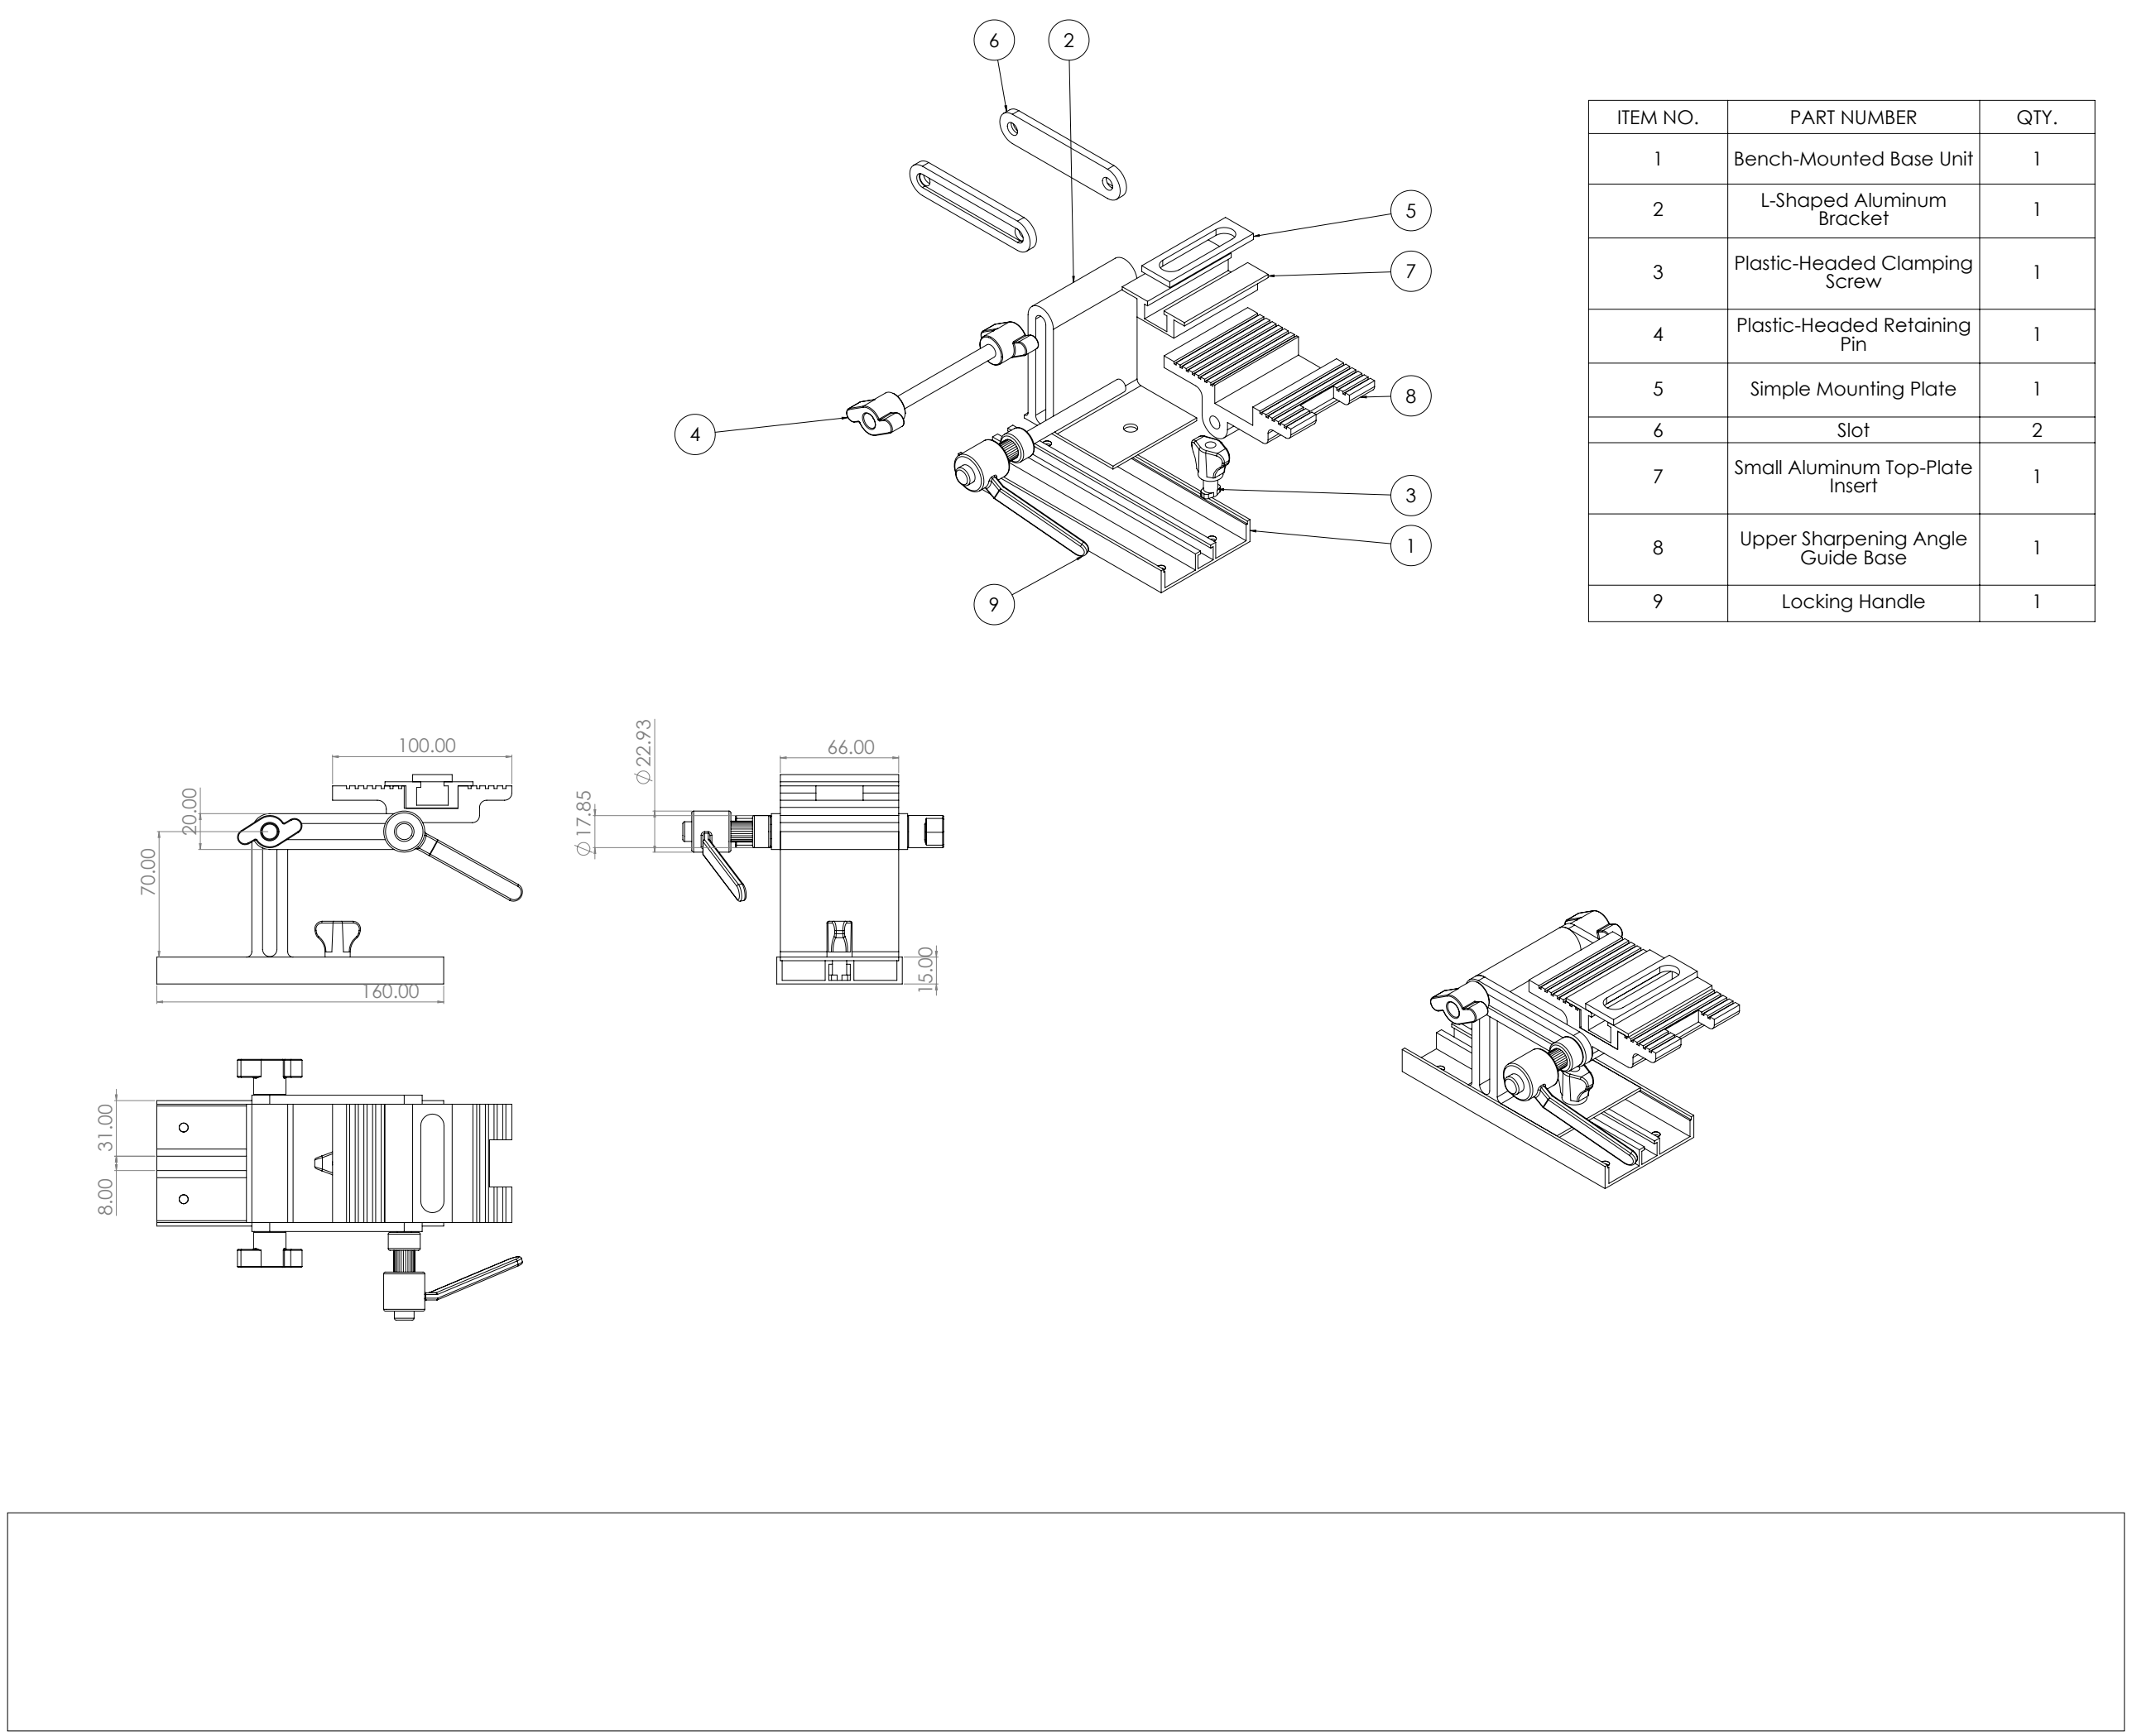
ISO-10303-21;
HEADER;
FILE_DESCRIPTION (('STEP AP214'),
    '1' );
FILE_NAME ('MAS-317',
    '2026-10-24T21:31:31',
    ( '' ),
    ( '' ),
    'SwSTEP 2.0',
    'SolidWorks 2025',
    '' );
FILE_SCHEMA (( 'AUTOMOTIVE_DESIGN' ));
ENDSEC;

DATA;
#1 = AXIS2_PLACEMENT_3D ( 'NONE', #1022, #12813, #2258 ) ;
#2 = CARTESIAN_POINT ( 'NONE',  ( 58.00000000000000711, -2.249290599286309256, 86.40005259842790508 ) ) ;
#3 = CARTESIAN_POINT ( 'NONE',  ( 58.00000000000000711, -2.249290599286309256, 86.40005259842790508 ) ) ;
#4 = EDGE_CURVE ( 'NONE', #12159, #10942, #11483, .T. ) ;
#5 = EDGE_LOOP ( 'NONE', ( #6099, #8745, #4266, #9000 ) ) ;
#6 = LINE ( 'NONE', #11694, #4610 ) ;
#7 = CARTESIAN_POINT ( 'NONE',  ( 64.16497654487091040, -11.91588057969686965, 72.65167857827074727 ) ) ;
#8 = EDGE_CURVE ( 'NONE', #12161, #11292, #4111, .T. ) ;
#9 = CARTESIAN_POINT ( 'NONE',  ( 27.62489819272141389, -52.24929059928630437, 4.899481419381555014 ) ) ;
#10 = CARTESIAN_POINT ( 'NONE',  ( 23.72005712271873890, -60.79495753911086098, 6.390225278796987318 ) ) ;
#11 = EDGE_LOOP ( 'NONE', ( #10298, #886, #9841, #4831, #11174, #11784, #1803, #163, #11627, #11601, #5374, #7472, #708, #12281, #12120, #14505 ) ) ;
#12 = EDGE_CURVE ( 'NONE', #11983, #7767, #13962, .T. ) ;
#13 = LINE ( 'NONE', #7011, #3647 ) ;
#14 = VECTOR ( 'NONE', #2004, 1000.000000000000000 ) ;
#15 = ORIENTED_EDGE ( 'NONE', *, *, #6036, .T. ) ;
#16 = CARTESIAN_POINT ( 'NONE',  ( 58.00000000000000711, -2.249290599286311032, 36.00000000000012079 ) ) ;
#17 = DIRECTION ( 'NONE',  ( -1.000000000000000000, 0.000000000000000000, 0.000000000000000000 ) ) ;
#18 = ADVANCED_FACE ( 'NONE', ( #1362 ), #5786, .T. ) ;
#19 = ADVANCED_FACE ( 'NONE', ( #7663 ), #4110, .F. ) ;
#20 = VERTEX_POINT ( 'NONE', #5429 ) ;
#21 =( NAMED_UNIT ( * ) PLANE_ANGLE_UNIT ( ) SI_UNIT ( $, .RADIAN. ) );
#22 = DIRECTION ( 'NONE',  ( 0.000000000000000000, 0.000000000000000000, -1.000000000000000000 ) ) ;
#23 = FACE_OUTER_BOUND ( 'NONE', #14250, .T. ) ;
#24 = ORIENTED_EDGE ( 'NONE', *, *, #9295, .T. ) ;
#25 = LINE ( 'NONE', #2406, #7510 ) ;
#26 = DIRECTION ( 'NONE',  ( -0.8746197071345572782, 0.4848096202550659650, 1.387778780781444256E-14 ) ) ;
#27 = ADVANCED_FACE ( 'NONE', ( #435 ), #1875, .T. ) ;
#28 = FACE_OUTER_BOUND ( 'NONE', #3772, .T. ) ;
#29 = DIRECTION ( 'NONE',  ( 1.000000000000000000, 0.000000000000000000, 0.000000000000000000 ) ) ;
#30 = EDGE_CURVE ( 'NONE', #1762, #13149, #4870, .T. ) ;
#31 = CARTESIAN_POINT ( 'NONE',  ( -24.73111225919155132, -6.857688092579577344, -47.70917337021941762 ) ) ;
#32 = FACE_OUTER_BOUND ( 'NONE', #11110, .T. ) ;
#33 = ADVANCED_FACE ( 'NONE', ( #12199 ), #9834, .F. ) ;
#34 = ORIENTED_EDGE ( 'NONE', *, *, #2571, .T. ) ;
#35 = CIRCLE ( 'NONE', #11822, 8.924024642120691908 ) ;
#36 = DIRECTION ( 'NONE',  ( 0.000000000000000000, 0.000000000000000000, 1.000000000000000000 ) ) ;
#37 = ORIENTED_EDGE ( 'NONE', *, *, #2232, .F. ) ;
#38 = FACE_OUTER_BOUND ( 'NONE', #6545, .T. ) ;
#39 = DIRECTION ( 'NONE',  ( -0.3020115420618247892, 0.1674077314120183957, -0.9384901064608620613 ) ) ;
#40 = CARTESIAN_POINT ( 'NONE',  ( 62.00000000000001421, -2.249290599286311032, -49.31370849898490150 ) ) ;
#41 = LINE ( 'NONE', #2497, #6085 ) ;
#42 = AXIS2_PLACEMENT_3D ( 'NONE', #10885, #14351, #11948 ) ;
#43 = CARTESIAN_POINT ( 'NONE',  ( 116.3214526938479025, -39.15081599364015119, 53.46824312087640863 ) ) ;
#44 = AXIS2_PLACEMENT_3D ( 'NONE', #5649, #10264, #10339 ) ;
#45 = CIRCLE ( 'NONE', #9384, 9.000000000000001776 ) ;
#46 = PLANE ( 'NONE',  #3626 ) ;
#47 = CARTESIAN_POINT ( 'NONE',  ( 46.91810375148135392, 21.75070940071322667, 139.1143251403882459 ) ) ;
#48 = CARTESIAN_POINT ( 'NONE',  ( -24.79038709231510040, -6.757381419356298657, 47.62582736825572738 ) ) ;
#49 = CARTESIAN_POINT ( 'NONE',  ( -2.016677571526633510E-15, 23.25070940071368497, -33.00000000000012790 ) ) ;
#50 = LINE ( 'NONE', #1350, #13702 ) ;
#51 = ORIENTED_EDGE ( 'NONE', *, *, #11161, .F. ) ;
#52 = CARTESIAN_POINT ( 'NONE',  ( 8.091875466796944139, -56.52532528994245808, 1.842181053809107238 ) ) ;
#53 = VECTOR ( 'NONE', #9034, 1000.000000000000000 ) ;
#54 = VECTOR ( 'NONE', #13573, 1000.000000000000000 ) ;
#55 = EDGE_CURVE ( 'NONE', #10251, #7651, #14932, .T. ) ;
#56 = VERTEX_POINT ( 'NONE', #6360 ) ;
#57 = LINE ( 'NONE', #11745, #6919 ) ;
#58 = VECTOR ( 'NONE', #2580, 1000.000000000000000 ) ;
#59 = VERTEX_POINT ( 'NONE', #10047 ) ;
#60 = VERTEX_POINT ( 'NONE', #14733 ) ;
#61 = CARTESIAN_POINT ( 'NONE',  ( 65.61438479068812057, -11.78561916032472823, 75.96106737140233633 ) ) ;
#62 = CARTESIAN_POINT ( 'NONE',  ( 114.6731053250840233, 21.75070940071369918, 139.1143251403882459 ) ) ;
#63 = DIRECTION ( 'NONE',  ( 0.000000000000000000, 1.734723475976817547E-15, -1.000000000000000000 ) ) ;
#64 = MECHANICAL_DESIGN_GEOMETRIC_PRESENTATION_REPRESENTATION (  '', ( #7176 ), #14543 ) ;
#65 = VERTEX_POINT ( 'NONE', #11047 ) ;
#66 = VECTOR ( 'NONE', #7622, 1000.000000000000000 ) ;
#67 = CARTESIAN_POINT ( 'NONE',  ( 8.466388902489018875, -58.63671300496866223, -1.826958383930360919 ) ) ;
#68 = PLANE ( 'NONE',  #7695 ) ;
#69 = LINE ( 'NONE', #10606, #11985 ) ;
#70 = CIRCLE ( 'NONE', #4772, 3.000000000000000888 ) ;
#71 = ORIENTED_EDGE ( 'NONE', *, *, #11240, .T. ) ;
#72 = VERTEX_POINT ( 'NONE', #721 ) ;
#73 = EDGE_CURVE ( 'NONE', #927, #9462, #501, .T. ) ;
#74 = EDGE_CURVE ( 'NONE', #5063, #10163, #11263, .T. ) ;
#75 = PLANE ( 'NONE',  #1648 ) ;
#76 = ORIENTED_EDGE ( 'NONE', *, *, #9899, .T. ) ;
#77 = VERTEX_POINT ( 'NONE', #4338 ) ;
#78 = CARTESIAN_POINT ( 'NONE',  ( 10.10272221478045296, -60.61171897230391892, -3.004288329735573804 ) ) ;
#79 = ORIENTED_EDGE ( 'NONE', *, *, #10646, .T. ) ;
#80 = CIRCLE ( 'NONE', #11854, 0.5000000000000000000 ) ;
#81 = VERTEX_POINT ( 'NONE', #9278 ) ;
#82 = B_SPLINE_CURVE_WITH_KNOTS ( 'NONE', 3,
 ( #2803, #3028, #1934, #12180, #8712, #1641, #3094, #13404, #11248, #10961, #410, #7643, #1857, #1791, #7796, #12259, #700, #6406 ),
 .UNSPECIFIED., .F., .F.,
 ( 4, 2, 2, 2, 2, 2, 2, 2, 4 ),
 ( 0.000000000000000000, 0.0007600084067931386217, 0.001520016813586277243, 0.002280025220379415865, 0.003040033627172554487, 0.003800042033965693108, 0.004560050440758831730, 0.005320058847551970352, 0.006080067254345108974 ),
 .UNSPECIFIED. ) ;
#83 = CARTESIAN_POINT ( 'NONE',  ( -24.54250511040913096, 2.674312581063694516, -47.50000000000008527 ) ) ;
#84 = DIRECTION ( 'NONE',  ( -0.000000000000000000, 0.000000000000000000, -1.000000000000000000 ) ) ;
#85 = ORIENTED_EDGE ( 'NONE', *, *, #4287, .T. ) ;
#86 = VECTOR ( 'NONE', #1332, 1000.000000000000000 ) ;
#87 = LINE ( 'NONE', #2465, #13317 ) ;
#88 = FACE_OUTER_BOUND ( 'NONE', #4233, .T. ) ;
#89 = ORIENTED_EDGE ( 'NONE', *, *, #5308, .T. ) ;
#90 = DIRECTION ( 'NONE',  ( 0.000000000000000000, 0.000000000000000000, -1.000000000000000000 ) ) ;
#91 = CARTESIAN_POINT ( 'NONE',  ( 32.77533487224304309, -57.91121052158847249, 2.751677492798574320 ) ) ;
#92 = APPLICATION_CONTEXT ( 'automotive_design' ) ;
#93 = CARTESIAN_POINT ( 'NONE',  ( -30.80945343098651890, -5.389243620311580329, -57.50000000000012079 ) ) ;
#94 = ORIENTED_EDGE ( 'NONE', *, *, #8937, .F. ) ;
#95 = VECTOR ( 'NONE', #9996, 1000.000000000000000 ) ;
#96 = DIRECTION ( 'NONE',  ( 0.9421718071228325497, 6.170304995646513309E-16, -0.3351302520855077849 ) ) ;
#97 = AXIS2_PLACEMENT_3D ( 'NONE', #6521, #12302, #1688 ) ;
#98 = ORIENTED_EDGE ( 'NONE', *, *, #8570, .T. ) ;
#99 = CARTESIAN_POINT ( 'NONE',  ( 40.00000000000001421, -72.24929059928631148, -32.99999999999982947 ) ) ;
#100 = DIRECTION ( 'NONE',  ( -0.8746197071345569451, 0.4848096202550666312, 0.000000000000000000 ) ) ;
#101 = ORIENTED_EDGE ( 'NONE', *, *, #8706, .F. ) ;
#102 = ORIENTED_EDGE ( 'NONE', *, *, #10358, .T. ) ;
#103 =( NAMED_UNIT ( * ) PLANE_ANGLE_UNIT ( ) SI_UNIT ( $, .RADIAN. ) );
#104 = CARTESIAN_POINT ( 'NONE',  ( 9.074528850127588697, -58.48798588983633095, 2.754379989674547780 ) ) ;
#105 = LINE ( 'NONE', #10640, #5976 ) ;
#106 = ORIENTED_EDGE ( 'NONE', *, *, #4616, .T. ) ;
#107 = CARTESIAN_POINT ( 'NONE',  ( -9.038486528834313916, 1.949452350488303454, -47.50000000626571506 ) ) ;
#108 = DIRECTION ( 'NONE',  ( 0.000000000000000000, 0.000000000000000000, 1.000000000000000000 ) ) ;
#109 = DIRECTION ( 'NONE',  ( 0.000000000000000000, 1.000000000000000000, 0.000000000000000000 ) ) ;
#110 = LINE ( 'NONE', #11941, #4147 ) ;
#111 = FACE_OUTER_BOUND ( 'NONE', #10692, .T. ) ;
#112 = EDGE_CURVE ( 'NONE', #12771, #10151, #4658, .T. ) ;
#113 = CARTESIAN_POINT ( 'NONE',  ( 33.37135420079148673, -55.04126158147273884, -2.748788379873860599 ) ) ;
#114 = ORIENTED_EDGE ( 'NONE', *, *, #14825, .F. ) ;
#115 = EDGE_LOOP ( 'NONE', ( #13949, #4522, #9265, #7527 ) ) ;
#116 = CARTESIAN_POINT ( 'NONE',  ( 0.000000000000000000, 21.75070940071363168, 33.00000000000012790 ) ) ;
#117 = VERTEX_POINT ( 'NONE', #8210 ) ;
#118 = LINE ( 'NONE', #8565, #1013 ) ;
#119 = CARTESIAN_POINT ( 'NONE',  ( -3.190546569013415379, 0.8906624217387615339, -57.50000000000012079 ) ) ;
#120 = LINE ( 'NONE', #8431, #11123 ) ;
#121 = CARTESIAN_POINT ( 'NONE',  ( 54.21883389619742388, -5.612936290787406968, 62.84860122826521689 ) ) ;
#122 = EDGE_CURVE ( 'NONE', #12222, #13012, #6096, .T. ) ;
#123 = ADVANCED_FACE ( 'NONE', ( #3273 ), #5820, .F. ) ;
#124 = CARTESIAN_POINT ( 'NONE',  ( 69.30309607900824176, -4.171217477998490075, 76.23845400177138742 ) ) ;
#125 = CARTESIAN_POINT ( 'NONE',  ( 13.86797143582180780, -68.67521603617343828, 4.260811380360699729 ) ) ;
#126 = DIRECTION ( 'NONE',  ( 0.000000000000000000, 0.000000000000000000, 1.000000000000000000 ) ) ;
#127 = CARTESIAN_POINT ( 'NONE',  ( -25.21252699837112132, -6.998437922861948657, 48.50000000000011369 ) ) ;
#128 = FACE_BOUND ( 'NONE', #8065, .T. ) ;
#129 = CARTESIAN_POINT ( 'NONE',  ( 30.58625090343030806, -52.41844408481608752, 2.861639392408844351 ) ) ;
#130 = ORIENTED_EDGE ( 'NONE', *, *, #11606, .T. ) ;
#131 = CARTESIAN_POINT ( 'NONE',  ( 20.86173033120691045, -53.24929059928630437, 0.000000000000000000 ) ) ;
#132 = ORIENTED_EDGE ( 'NONE', *, *, #1705, .F. ) ;
#133 = DIRECTION ( 'NONE',  ( 1.000000000000000000, 0.000000000000000000, 0.000000000000000000 ) ) ;
#134 = ORIENTED_EDGE ( 'NONE', *, *, #9339, .T. ) ;
#135 = ORIENTED_EDGE ( 'NONE', *, *, #2741, .T. ) ;
#136 = CARTESIAN_POINT ( 'NONE',  ( 64.12616288941416087, -11.93994285747185913, 75.47114622899779590 ) ) ;
#137 = CARTESIAN_POINT ( 'NONE',  ( 65.80512781895316721, -6.575743597179694255, 39.50000000000012790 ) ) ;
#138 = CARTESIAN_POINT ( 'NONE',  ( 48.00000000000000000, -2.249290599286307479, 139.1143251403882459 ) ) ;
#139 = CARTESIAN_POINT ( 'NONE',  ( 9.123957934261133218, -53.72645478541605257, 3.103403305059656336 ) ) ;
#140 = ADVANCED_FACE ( 'NONE', ( #6968 ), #10511, .T. ) ;
#141 = CARTESIAN_POINT ( 'NONE',  ( 59.31076468612580754, 2.638779099491020297, 60.61639468829817190 ) ) ;
#142 = CARTESIAN_POINT ( 'NONE',  ( 67.15257324181105503, -7.322644791425994448, 61.61639468829817190 ) ) ;
#143 = VERTEX_POINT ( 'NONE', #9046 ) ;
#144 = CARTESIAN_POINT ( 'NONE',  ( 65.51787304867481510, -10.90583193546819274, 77.18393887567587797 ) ) ;
#145 = ORIENTED_EDGE ( 'NONE', *, *, #4688, .T. ) ;
#146 = DIRECTION ( 'NONE',  ( -0.9744556954135545901, 0.2245798247307304318, 0.000000000000000000 ) ) ;
#147 = ORIENTED_EDGE ( 'NONE', *, *, #2886, .F. ) ;
#148 = LINE ( 'NONE', #14233, #12794 ) ;
#149 = AXIS2_PLACEMENT_3D ( 'NONE', #12314, #13325, #4001 ) ;
#150 = ORIENTED_EDGE ( 'NONE', *, *, #12236, .T. ) ;
#151 = CARTESIAN_POINT ( 'NONE',  ( -22.13891797369473480, 5.141277655368648780, -48.38337049880507834 ) ) ;
#152 = CARTESIAN_POINT ( 'NONE',  ( 65.93900958890544928, -0.9331851346922672708, 76.19766410831374515 ) ) ;
#153 = VERTEX_POINT ( 'NONE', #5752 ) ;
#154 = DIRECTION ( 'NONE',  ( -0.000000000000000000, 1.000000000000000000, -0.000000000000000000 ) ) ;
#155 = LINE ( 'NONE', #2612, #2752 ) ;
#156 = EDGE_LOOP ( 'NONE', ( #7728, #5694, #9406, #597 ) ) ;
#157 = EDGE_CURVE ( 'NONE', #531, #1580, #7972, .T. ) ;
#158 = ADVANCED_FACE ( 'NONE', ( #10353 ), #436, .F. ) ;
#159 = TOROIDAL_SURFACE ( 'NONE', #9985, 10.46463184759104870, 1.000000000000000000 ) ;
#160 = DIRECTION ( 'NONE',  ( -0.000000000000000000, -0.000000000000000000, -1.000000000000000000 ) ) ;
#161 = CARTESIAN_POINT ( 'NONE',  ( 42.07846078193830408, 21.75070940071319114, 139.1143251403882459 ) ) ;
#162 = DIRECTION ( 'NONE',  ( 0.000000000000000000, 0.000000000000000000, 1.000000000000000000 ) ) ;
#163 = ORIENTED_EDGE ( 'NONE', *, *, #14073, .T. ) ;
#164 = CARTESIAN_POINT ( 'NONE',  ( -24.34296084301338681, 2.966536634491813818, 47.54128347412125066 ) ) ;
#165 = EDGE_CURVE ( 'NONE', #11054, #3062, #11494, .T. ) ;
#166 = VERTEX_POINT ( 'NONE', #3346 ) ;
#167 = DIRECTION ( 'NONE',  ( -1.000000000000000000, 0.000000000000000000, 0.000000000000000000 ) ) ;
#168 =( NAMED_UNIT ( * ) PLANE_ANGLE_UNIT ( ) SI_UNIT ( $, .RADIAN. ) );
#169 = AXIS2_PLACEMENT_3D ( 'NONE', #4841, #13010, #2308 ) ;
#170 = VERTEX_POINT ( 'NONE', #13972 ) ;
#171 = VECTOR ( 'NONE', #13826, 1000.000000000000000 ) ;
#172 = LINE ( 'NONE', #1320, #11742 ) ;
#173 = CARTESIAN_POINT ( 'NONE',  ( 29.24198010098110245, -64.22824823034754615, 3.135769320951033112 ) ) ;
#174 = EDGE_CURVE ( 'NONE', #2378, #7934, #12219, .T. ) ;
#175 = CARTESIAN_POINT ( 'NONE',  ( -9.097850607046364502, 2.059891325575069043, -47.52616914649232172 ) ) ;
#176 = CARTESIAN_POINT ( 'NONE',  ( 13.73779544508787431, -66.12426320349668174, 4.110478850042866839 ) ) ;
#177 = AXIS2_PLACEMENT_3D ( 'NONE', #1271, #10901, #2354 ) ;
#178 = LINE ( 'NONE', #7254, #6578 ) ;
#179 = FACE_OUTER_BOUND ( 'NONE', #4257, .T. ) ;
#180 = CARTESIAN_POINT ( 'NONE',  ( 33.55553634841081845, -55.70626543767114214, 1.910065177037574946 ) ) ;
#181 = CIRCLE ( 'NONE', #13427, 4.505436745857433145 ) ;
#182 = FACE_OUTER_BOUND ( 'NONE', #8671, .T. ) ;
#183 = CIRCLE ( 'NONE', #7797, 6.484807146443463566 ) ;
#184 = ORIENTED_EDGE ( 'NONE', *, *, #4181, .F. ) ;
#185 = CARTESIAN_POINT ( 'NONE',  ( 121.8459904851758893, -37.63970102501964021, 53.02550872668530246 ) ) ;
#186 = EDGE_LOOP ( 'NONE', ( #1865, #4805, #14383, #1234 ) ) ;
#187 = CARTESIAN_POINT ( 'NONE',  ( 67.21328690825531282, 25.52935533987996664, 84.20452624982236500 ) ) ;
#188 = CARTESIAN_POINT ( 'NONE',  ( 18.24487436548682240, -53.24929059928630437, 6.492462156583986399 ) ) ;
#189 = PRODUCT_DEFINITION_FORMATION_WITH_SPECIFIED_SOURCE ( 'ANY', '', #5935, .NOT_KNOWN. ) ;
#190 = DIRECTION ( 'NONE',  ( -1.000000000000000000, -0.000000000000000000, -0.000000000000000000 ) ) ;
#191 = DIRECTION ( 'NONE',  ( 0.000000000000000000, 0.000000000000000000, 1.000000000000000000 ) ) ;
#192 = CIRCLE ( 'NONE', #14918, 0.7892041907098250597 ) ;
#193 = TOROIDAL_SURFACE ( 'NONE', #8776, 5.165819364273509073, 0.5000000000000000000 ) ;
#194 = CARTESIAN_POINT ( 'NONE',  ( -16.99999999999998579, -2.249290599286303927, 33.00000000000012790 ) ) ;
#195 = CARTESIAN_POINT ( 'NONE',  ( 65.61529858912808777, -10.82031860958136704, 71.19766410831375936 ) ) ;
#196 = EDGE_CURVE ( 'NONE', #211, #4051, #4578, .T. ) ;
#197 = DIRECTION ( 'NONE',  ( 1.000000000000000000, 0.000000000000000000, 0.000000000000000000 ) ) ;
#198 = CARTESIAN_POINT ( 'NONE',  ( -25.01741698508091005, -6.338425579613558014, 48.00000000000010658 ) ) ;
#199 = AXIS2_PLACEMENT_3D ( 'NONE', #2893, #5282, #2974 ) ;
#200 = CLOSED_SHELL ( 'NONE', ( #3830, #2727, #245, #8105, #11848, #11362, #3505, #1082, #828, #2082, #3069, #6755, #8169, #6132, #6771, #8839, #9223 ) ) ;
#201 = CARTESIAN_POINT ( 'NONE',  ( 32.69801279946867112, -53.84541978742783641, 3.062363702218897643 ) ) ;
#202 = ADVANCED_FACE ( 'NONE', ( #3509 ), #12825, .F. ) ;
#203 = VECTOR ( 'NONE', #10665, 1000.000000000000000 ) ;
#204 = ORIENTED_EDGE ( 'NONE', *, *, #247, .F. ) ;
#205 = ADVANCED_FACE ( 'NONE', ( #8045 ), #8050, .F. ) ;
#206 = AXIS2_PLACEMENT_3D ( 'NONE', #6103, #12884, #8338 ) ;
#207 = EDGE_CURVE ( 'NONE', #5032, #7204, #4344, .T. ) ;
#208 = DIRECTION ( 'NONE',  ( -2.102695122396130409E-16, 0.000000000000000000, -1.000000000000000000 ) ) ;
#209 = ORIENTED_EDGE ( 'NONE', *, *, #14302, .F. ) ;
#210 = CARTESIAN_POINT ( 'NONE',  ( 1.004339113574583608, 0.8906624217387615339, -48.00000000000012079 ) ) ;
#211 = VERTEX_POINT ( 'NONE', #3190 ) ;
#212 = PLANE ( 'NONE',  #10140 ) ;
#213 = DIRECTION ( 'NONE',  ( 0.000000000000000000, 0.000000000000000000, -1.000000000000000000 ) ) ;
#214 = EDGE_CURVE ( 'NONE', #14442, #11277, #7315, .T. ) ;
#215 = CIRCLE ( 'NONE', #445, 0.5000000000000000000 ) ;
#216 = LINE ( 'NONE', #3742, #12117 ) ;
#217 = DIRECTION ( 'NONE',  ( -0.000000000000000000, 0.000000000000000000, 1.000000000000000000 ) ) ;
#218 = PLANE ( 'NONE',  #1793 ) ;
#219 = DIRECTION ( 'NONE',  ( 0.8420378618367728718, 0.5394184268574404584, -0.000000000000000000 ) ) ;
#220 = ORIENTED_EDGE ( 'NONE', *, *, #12965, .T. ) ;
#221 = EDGE_LOOP ( 'NONE', ( #14150, #12830, #6180, #1820 ) ) ;
#222 = EDGE_CURVE ( 'NONE', #13907, #15116, #14885, .T. ) ;
#223 = DIRECTION ( 'NONE',  ( 9.912705577010325549E-17, -1.734723475976817547E-15, 1.000000000000000000 ) ) ;
#224 = ORIENTED_EDGE ( 'NONE', *, *, #5040, .T. ) ;
#225 = ORIENTED_EDGE ( 'NONE', *, *, #12393, .F. ) ;
#226 = CYLINDRICAL_SURFACE ( 'NONE', #7156, 10.15857703477299978 ) ;
#227 = ORIENTED_EDGE ( 'NONE', *, *, #14224, .F. ) ;
#228 = CARTESIAN_POINT ( 'NONE',  ( 12.36791015745245836, -52.24929059928630437, 3.199931146564424012 ) ) ;
#229 = AXIS2_PLACEMENT_3D ( 'NONE', #14012, #3468, #10624 ) ;
#230 = EDGE_CURVE ( 'NONE', #13103, #13525, #1896, .T. ) ;
#231 = EDGE_LOOP ( 'NONE', ( #10918, #12061, #5408, #5048 ) ) ;
#232 = DIRECTION ( 'NONE',  ( 0.8746197071345569451, -0.4848096202550666312, 0.000000000000000000 ) ) ;
#233 = CARTESIAN_POINT ( 'NONE',  ( 63.00747169918385993, -1.516790343742004055, 62.84860122826521689 ) ) ;
#234 = ORIENTED_EDGE ( 'NONE', *, *, #174, .T. ) ;
#235 = LINE ( 'NONE', #14317, #9148 ) ;
#236 = CARTESIAN_POINT ( 'NONE',  ( 118.0000000000000568, 2.046973701652633381E-13, 13.14990448602693007 ) ) ;
#237 = ORIENTED_EDGE ( 'NONE', *, *, #6908, .T. ) ;
#238 = VECTOR ( 'NONE', #7025, 1000.000000000000000 ) ;
#239 = CARTESIAN_POINT ( 'NONE',  ( 24.10826840236109803, -69.39711819508849544, -6.201611931792124111 ) ) ;
#240 = CARTESIAN_POINT ( 'NONE',  ( 48.00000000000000711, 10.25070940071368497, -33.00000000000012790 ) ) ;
#241 = CARTESIAN_POINT ( 'NONE',  ( -28.95977857253349796, -8.587818791446737876, 48.00000000000012079 ) ) ;
#242 = EDGE_CURVE ( 'NONE', #604, #9712, #875, .T. ) ;
#243 = ORIENTED_EDGE ( 'NONE', *, *, #2367, .F. ) ;
#244 = CARTESIAN_POINT ( 'NONE',  ( -23.91311688008704905, 3.524160940036151324, 47.66502101098827637 ) ) ;
#245 = ADVANCED_FACE ( 'NONE', ( #4003, #4739 ), #46, .F. ) ;
#246 = VERTEX_POINT ( 'NONE', #9730 ) ;
#247 = EDGE_CURVE ( 'NONE', #8031, #13187, #10874, .T. ) ;
#248 = CARTESIAN_POINT ( 'NONE',  ( 53.45023817967523172, -5.433760736713491468, 48.51982618741349285 ) ) ;
#249 = CARTESIAN_POINT ( 'NONE',  ( 104.0000000000000426, 15.25070940071369563, -33.00000000000012790 ) ) ;
#250 = CIRCLE ( 'NONE', #10335, 1.000000000000000888 ) ;
#251 = VERTEX_POINT ( 'NONE', #11733 ) ;
#252 = APPLICATION_PROTOCOL_DEFINITION ( 'draft international standard', 'automotive_design', 1998, #5158 ) ;
#253 = CARTESIAN_POINT ( 'NONE',  ( -10.99067925302910176, -8.982598353005794678, -48.14374739243442747 ) ) ;
#254 = FACE_OUTER_BOUND ( 'NONE', #221, .T. ) ;
#255 = DIRECTION ( 'NONE',  ( 0.000000000000000000, 0.000000000000000000, -1.000000000000000000 ) ) ;
#256 = CARTESIAN_POINT ( 'NONE',  ( 9.949736305181877682, -63.13800426656748499, 2.713090553606876121 ) ) ;
#257 = DIRECTION ( 'NONE',  ( 0.000000000000000000, 1.000000000000000000, -0.000000000000000000 ) ) ;
#258 = CARTESIAN_POINT ( 'NONE',  ( 27.33382790127958728, -69.39711819508849544, 4.502057496415716287 ) ) ;
#259 = DIRECTION ( 'NONE',  ( 0.000000000000000000, 0.000000000000000000, 1.000000000000000000 ) ) ;
#260 = AXIS2_PLACEMENT_3D ( 'NONE', #10023, #5325, #2943 ) ;
#261 = CARTESIAN_POINT ( 'NONE',  ( 31.94014848486111191, -53.10528739703779877, -3.364210193422788375 ) ) ;
#262 = ADVANCED_FACE ( 'NONE', ( #2849 ), #1628, .F. ) ;
#263 = CARTESIAN_POINT ( 'NONE',  ( -6.999999999999985789, -2.249290599286299930, -115.4621125123531442 ) ) ;
#264 = EDGE_CURVE ( 'NONE', #12856, #5130, #362, .T. ) ;
#265 = ORIENTED_EDGE ( 'NONE', *, *, #2651, .T. ) ;
#266 = DIRECTION ( 'NONE',  ( -0.000000000000000000, -0.000000000000000000, -1.000000000000000000 ) ) ;
#267 = FACE_OUTER_BOUND ( 'NONE', #14593, .T. ) ;
#268 = DIRECTION ( 'NONE',  ( -0.8746197071345569451, 0.4848096202550666312, 0.000000000000000000 ) ) ;
#269 = ORIENTED_EDGE ( 'NONE', *, *, #14642, .F. ) ;
#270 = VECTOR ( 'NONE', #1744, 1000.000000000000000 ) ;
#271 = CARTESIAN_POINT ( 'NONE',  ( 69.97972559857380759, -3.172990593254280789, 75.19766410831374515 ) ) ;
#272 = FACE_OUTER_BOUND ( 'NONE', #12686, .T. ) ;
#273 = DIRECTION ( 'NONE',  ( -0.000000000000000000, -0.000000000000000000, -1.000000000000000000 ) ) ;
#274 = CARTESIAN_POINT ( 'NONE',  ( -24.96483633670257873, -6.441926561070030033, 48.01692658285762150 ) ) ;
#275 = AXIS2_PLACEMENT_3D ( 'NONE', #4169, #10894, #7496 ) ;
#276 = CARTESIAN_POINT ( 'NONE',  ( 31.87918814257875155, -54.14181112192009238, 3.331498666157771016 ) ) ;
#277 = ORIENTED_EDGE ( 'NONE', *, *, #11092, .F. ) ;
#278 = DIRECTION ( 'NONE',  ( 0.000000000000000000, 0.000000000000000000, -1.000000000000000000 ) ) ;
#279 = ORIENTED_EDGE ( 'NONE', *, *, #8747, .F. ) ;
#280 = LINE ( 'NONE', #11038, #4450 ) ;
#281 = ORIENTED_EDGE ( 'NONE', *, *, #7345, .T. ) ;
#282 = AXIS2_PLACEMENT_3D ( 'NONE', #9055, #1887, #6818 ) ;
#283 = CARTESIAN_POINT ( 'NONE',  ( 64.80908095809924419, -11.48972663575131392, 75.86800894915671734 ) ) ;
#284 = EDGE_CURVE ( 'NONE', #12776, #11451, #5880, .T. ) ;
#285 = DIRECTION ( 'NONE',  ( 0.8746197071345571672, -0.4848096202550661871, 0.000000000000000000 ) ) ;
#286 = VECTOR ( 'NONE', #5569, 1000.000000000000000 ) ;
#287 = CIRCLE ( 'NONE', #2244, 4.000000000000000000 ) ;
#288 = DIRECTION ( 'NONE',  ( 0.000000000000000000, -0.000000000000000000, -1.000000000000000000 ) ) ;
#289 = CARTESIAN_POINT ( 'NONE',  ( 9.168176149879958103, -53.68423722363644401, 2.283982087543965367 ) ) ;
#290 = CARTESIAN_POINT ( 'NONE',  ( -25.46282903980762669, -6.565599745187292946, 47.50000000000012079 ) ) ;
#291 = VECTOR ( 'NONE', #10970, 1000.000000000000000 ) ;
#292 = EDGE_CURVE ( 'NONE', #5596, #3737, #9002, .T. ) ;
#293 = AXIS2_PLACEMENT_3D ( 'NONE', #12680, #6824, #7986 ) ;
#294 = DIRECTION ( 'NONE',  ( -0.8746197071345569451, 0.4848096202550666312, 0.000000000000000000 ) ) ;
#295 = ADVANCED_FACE ( 'NONE', ( #10164 ), #9788, .F. ) ;
#296 = ORIENTED_EDGE ( 'NONE', *, *, #1661, .T. ) ;
#297 = TOROIDAL_SURFACE ( 'NONE', #10121, 4.496540510819672321, 1.000000000000000000 ) ;
#298 = VERTEX_POINT ( 'NONE', #5547 ) ;
#299 = DIRECTION ( 'NONE',  ( 0.000000000000000000, 1.000000000000000000, 0.000000000000000000 ) ) ;
#300 = ORIENTED_EDGE ( 'NONE', *, *, #12912, .T. ) ;
#301 = CARTESIAN_POINT ( 'NONE',  ( 13.63336148250377100, -65.27414832489905905, 4.302972696997120039 ) ) ;
#302 = VERTEX_POINT ( 'NONE', #4387 ) ;
#303 = FACE_OUTER_BOUND ( 'NONE', #6423, .T. ) ;
#304 = VERTEX_POINT ( 'NONE', #7858 ) ;
#305 = DIRECTION ( 'NONE',  ( 0.000000000000000000, 0.000000000000000000, 1.000000000000000000 ) ) ;
#306 = DIRECTION ( 'NONE',  ( -0.000000000000000000, 0.000000000000000000, -1.000000000000000000 ) ) ;
#307 = VERTEX_POINT ( 'NONE', #9085 ) ;
#308 = AXIS2_PLACEMENT_3D ( 'NONE', #9751, #6496, #11257 ) ;
#309 = ADVANCED_FACE ( 'NONE', ( #12548, #6765 ), #13774, .T. ) ;
#310 = CIRCLE ( 'NONE', #8176, 4.665819364273509073 ) ;
#311 = EDGE_CURVE ( 'NONE', #2576, #7654, #192, .T. ) ;
#312 = CARTESIAN_POINT ( 'NONE',  ( 29.48535251946101710, -62.76259148841303670, -3.786770376139251937 ) ) ;
#313 = CARTESIAN_POINT ( 'NONE',  ( 65.00000000000001421, -85.24929059928631148, 19.99999999999999645 ) ) ;
#314 = ORIENTED_EDGE ( 'NONE', *, *, #11289, .T. ) ;
#315 = PLANE ( 'NONE',  #10049 ) ;
#316 = CARTESIAN_POINT ( 'NONE',  ( 32.90197589884652274, -57.33450387999030795, 2.749014434309885235 ) ) ;
#317 = ORIENTED_EDGE ( 'NONE', *, *, #10206, .F. ) ;
#318 = VECTOR ( 'NONE', #6465, 1000.000000000000000 ) ;
#319 = FACE_OUTER_BOUND ( 'NONE', #4555, .T. ) ;
#320 = VECTOR ( 'NONE', #7998, 1000.000000000000000 ) ;
#321 = ORIENTED_EDGE ( 'NONE', *, *, #14732, .T. ) ;
#322 = VERTEX_POINT ( 'NONE', #10317 ) ;
#323 = CARTESIAN_POINT ( 'NONE',  ( -16.99999999999998579, -2.249290599286303927, 38.00000000000012079 ) ) ;
#324 = ORIENTED_EDGE ( 'NONE', *, *, #7653, .T. ) ;
#325 = ORIENTED_EDGE ( 'NONE', *, *, #6325, .F. ) ;
#326 = APPLICATION_PROTOCOL_DEFINITION ( 'draft international standard', 'automotive_design', 1998, #2511 ) ;
#327 = CYLINDRICAL_SURFACE ( 'NONE', #4362, 1.000000000000005329 ) ;
#328 = CARTESIAN_POINT ( 'NONE',  ( 62.50543674585744469, -2.249290599286311032, 36.00000000000012079 ) ) ;
#329 = CARTESIAN_POINT ( 'NONE',  ( -9.191242442328487527, 2.249476921181321476, -48.36238429206942868 ) ) ;
#330 = CARTESIAN_POINT ( 'NONE',  ( 13.85027004230004444, -68.05254135517340330, 4.069129116404105240 ) ) ;
#331 = CARTESIAN_POINT ( 'NONE',  ( 32.35433946108159375, -60.80954383512729322, 1.970170733381438222 ) ) ;
#332 = VECTOR ( 'NONE', #3067, 1000.000000000000000 ) ;
#333 = CARTESIAN_POINT ( 'NONE',  ( 12.03298173962126683, -53.28399145779480506, 4.141535524925028078 ) ) ;
#334 = DIRECTION ( 'NONE',  ( -0.8746197071345570562, 0.4848096202550662981, 0.000000000000000000 ) ) ;
#335 = EDGE_CURVE ( 'NONE', #11258, #1446, #2933, .T. ) ;
#336 = CIRCLE ( 'NONE', #6243, 3.694885682587998765 ) ;
#337 = CARTESIAN_POINT ( 'NONE',  ( -26.99999999999998224, -72.24929059928645358, -33.00000000000000000 ) ) ;
#338 = CARTESIAN_POINT ( 'NONE',  ( 32.37230692610057758, -54.69057383521065674, -3.126673503084364203 ) ) ;
#339 = EDGE_CURVE ( 'NONE', #4676, #369, #5590, .T. ) ;
#340 = DIRECTION ( 'NONE',  ( 0.000000000000000000, 0.000000000000000000, 1.000000000000000000 ) ) ;
#341 = VERTEX_POINT ( 'NONE', #685 ) ;
#342 = DIRECTION ( 'NONE',  ( 0.000000000000000000, 0.000000000000000000, 1.000000000000000000 ) ) ;
#343 = DIRECTION ( 'NONE',  ( 0.9744556954135530358, -0.2245798247307378148, 0.000000000000000000 ) ) ;
#344 = VECTOR ( 'NONE', #582, 1000.000000000000000 ) ;
#345 = DIRECTION ( 'NONE',  ( 0.000000000000000000, -0.000000000000000000, -1.000000000000000000 ) ) ;
#346 = LINE ( 'NONE', #12902, #10507 ) ;
#347 = CARTESIAN_POINT ( 'NONE',  ( 69.46221311448613278, -2.886128737383383935, 75.38059407619712715 ) ) ;
#348 = CARTESIAN_POINT ( 'NONE',  ( 96.29968967959054282, 25.52935533987996664, 33.00000000000012790 ) ) ;
#349 = EDGE_CURVE ( 'NONE', #13079, #8396, #2395, .T. ) ;
#350 = DIRECTION ( 'NONE',  ( -0.8656763553493062036, -0.5006040828730242698, -0.000000000000000000 ) ) ;
#351 = EDGE_CURVE ( 'NONE', #1115, #11167, #14092, .T. ) ;
#352 = CYLINDRICAL_SURFACE ( 'NONE', #8410, 4.000000000000003553 ) ;
#353 = ORIENTED_EDGE ( 'NONE', *, *, #9943, .F. ) ;
#354 = CARTESIAN_POINT ( 'NONE',  ( -29.99999999999998579, -72.24929059928631148, 33.00000000000000000 ) ) ;
#355 = VERTEX_POINT ( 'NONE', #12871 ) ;
#356 = CARTESIAN_POINT ( 'NONE',  ( -25.46282903980762669, -6.565599745187292946, 48.00000000000012079 ) ) ;
#357 = ORIENTED_EDGE ( 'NONE', *, *, #11069, .T. ) ;
#358 = VERTEX_POINT ( 'NONE', #2315 ) ;
#360 = ORIENTED_EDGE ( 'NONE', *, *, #2072, .T. ) ;
#359 = DIRECTION ( 'NONE',  ( 1.000000000000000000, 0.000000000000000000, 0.000000000000000000 ) ) ;
#361 = CARTESIAN_POINT ( 'NONE',  ( -32.80254285330622110, -2.278009980413880697, -48.50000000000012079 ) ) ;
#362 = B_SPLINE_CURVE_WITH_KNOTS ( 'NONE', 3,
 ( #5026, #12249, #5902, #7328, #3856, #12016, #331, #8559, #13257, #9804 ),
 .UNSPECIFIED., .F., .F.,
 ( 4, 2, 2, 2, 4 ),
 ( 0.000000000000000000, 0.0006693228878568694860, 0.001338645775713738972, 0.002007968663570608350, 0.002677291551427477944 ),
 .UNSPECIFIED. ) ;
#363 = DIRECTION ( 'NONE',  ( 0.000000000000000000, 0.000000000000000000, 1.000000000000000000 ) ) ;
#364 = EDGE_CURVE ( 'NONE', #14069, #12214, #5110, .T. ) ;
#365 = ORIENTED_EDGE ( 'NONE', *, *, #10647, .T. ) ;
#366 = DIRECTION ( 'NONE',  ( 0.000000000000000000, 1.000000000000000000, 2.081668171172168119E-15 ) ) ;
#367 = DIRECTION ( 'NONE',  ( 0.000000000000000000, 0.000000000000000000, 1.000000000000000000 ) ) ;
#368 = CARTESIAN_POINT ( 'NONE',  ( -2.688903428702175252E-15, 23.25070940071368142, 33.00000000000012790 ) ) ;
#369 = VERTEX_POINT ( 'NONE', #6019 ) ;
#370 = CARTESIAN_POINT ( 'NONE',  ( 0.000000000000000000, 21.75070940071329417, 139.1143251403882459 ) ) ;
#371 = ORIENTED_EDGE ( 'NONE', *, *, #10491, .F. ) ;
#372 = DIRECTION ( 'NONE',  ( 1.000000000000000000, 0.000000000000000000, 0.000000000000000000 ) ) ;
#373 = ORIENTED_EDGE ( 'NONE', *, *, #13891, .T. ) ;
#374 = CARTESIAN_POINT ( 'NONE',  ( 31.12893072306533071, -61.89517205450268733, 2.369674354374375458 ) ) ;
#375 = ORIENTED_EDGE ( 'NONE', *, *, #2546, .T. ) ;
#376 = DIRECTION ( 'NONE',  ( -0.000000000000000000, -0.000000000000000000, -1.000000000000000000 ) ) ;
#377 = DIRECTION ( 'NONE',  ( 0.8746197071345570562, -0.4848096202550665756, 0.000000000000000000 ) ) ;
#378 = EDGE_LOOP ( 'NONE', ( #12434, #11503, #11290, #1533 ) ) ;
#379 = LINE ( 'NONE', #14467, #12326 ) ;
#380 = ORIENTED_EDGE ( 'NONE', *, *, #7068, .T. ) ;
#381 = CYLINDRICAL_SURFACE ( 'NONE', #9577, 11.46463184759105403 ) ;
#382 = CARTESIAN_POINT ( 'NONE',  ( 50.19487218104683990, 2.077162398607073968, 82.40005259842790508 ) ) ;
#383 = CARTESIAN_POINT ( 'NONE',  ( 19.97461805067967688, 0.000000000000000000, -4.000000000000000888 ) ) ;
#384 = VERTEX_POINT ( 'NONE', #5940 ) ;
#385 = CARTESIAN_POINT ( 'NONE',  ( -24.57377864815406099, 2.621914368698142983, 47.92899112040971943 ) ) ;
#386 = EDGE_CURVE ( 'NONE', #5046, #7147, #1076, .T. ) ;
#387 = EDGE_CURVE ( 'NONE', #550, #2283, #6562, .T. ) ;
#388 = EDGE_CURVE ( 'NONE', #5785, #8918, #8303, .T. ) ;
#389 = ORIENTED_EDGE ( 'NONE', *, *, #387, .F. ) ;
#390 = FACE_OUTER_BOUND ( 'NONE', #10750, .T. ) ;
#391 = ORIENTED_EDGE ( 'NONE', *, *, #15115, .F. ) ;
#392 = APPLICATION_PROTOCOL_DEFINITION ( 'draft international standard', 'automotive_design', 1998, #8716 ) ;
#393 = DIRECTION ( 'NONE',  ( 1.000000000000000000, 0.000000000000000000, 0.000000000000000000 ) ) ;
#394 = DIRECTION ( 'NONE',  ( 1.000000000000000000, -9.251858538542971581E-17, 0.000000000000000000 ) ) ;
#395 = EDGE_CURVE ( 'NONE', #2944, #14405, #10471, .T. ) ;
#396 = CARTESIAN_POINT ( 'NONE',  ( -10.31873516982594907, -8.289185193041582522, -47.74939190649462972 ) ) ;
#397 = AXIS2_PLACEMENT_3D ( 'NONE', #6924, #8082, #15007 ) ;
#398 = CARTESIAN_POINT ( 'NONE',  ( 114.0000000000000284, 15.25070940071369563, 139.1143251403882459 ) ) ;
#399 = CARTESIAN_POINT ( 'NONE',  ( 31.74193665722908264, -52.96285630328479499, 2.532360049841041683 ) ) ;
#400 = CARTESIAN_POINT ( 'NONE',  ( 80.00000000000001421, -72.24929059928631148, -32.99999999999999289 ) ) ;
#401 = PRODUCT_DEFINITION_SHAPE ( 'NONE', 'NONE',  #15236 ) ;
#402 = AXIS2_PLACEMENT_3D ( 'NONE', #1965, #6663, #11352 ) ;
#403 = CARTESIAN_POINT ( 'NONE',  ( -8.729485970062036415, 2.417371407811747197, 48.19241902544784750 ) ) ;
#404 = VERTEX_POINT ( 'NONE', #7006 ) ;
#405 = CARTESIAN_POINT ( 'NONE',  ( -16.99999999999998579, -12.24929059928630437, 38.00000000000012079 ) ) ;
#406 = CARTESIAN_POINT ( 'NONE',  ( 57.51704887355756313, 3.283153786997079049, 60.61639468829817190 ) ) ;
#407 = DIRECTION ( 'NONE',  ( 0.000000000000000000, 0.000000000000000000, 1.000000000000000000 ) ) ;
#408 = CYLINDRICAL_SURFACE ( 'NONE', #2891, 1.000000000000000888 ) ;
#409 = EDGE_CURVE ( 'NONE', #4378, #2618, #11532, .T. ) ;
#410 = CARTESIAN_POINT ( 'NONE',  ( 9.212626894557791601, -54.90380519981211194, 3.064473585392920363 ) ) ;
#411 = FACE_OUTER_BOUND ( 'NONE', #3533, .T. ) ;
#412 = AXIS2_PLACEMENT_3D ( 'NONE', #11507, #13599, #12438 ) ;
#413 = AXIS2_PLACEMENT_3D ( 'NONE', #11900, #10826, #1359 ) ;
#414 = CARTESIAN_POINT ( 'NONE',  ( 27.86173033120691045, -69.39711819508849544, -3.619682905202609380 ) ) ;
#415 = CARTESIAN_POINT ( 'NONE',  ( -25.21252699939434194, -6.998437923453657561, -48.43453164808065736 ) ) ;
#416 = CIRCLE ( 'NONE', #10992, 0.7892041907098262810 ) ;
#417 =( GEOMETRIC_REPRESENTATION_CONTEXT ( 3 ) GLOBAL_UNCERTAINTY_ASSIGNED_CONTEXT ( ( #1045 ) ) GLOBAL_UNIT_ASSIGNED_CONTEXT ( ( #9181, #13866, #10252 ) ) REPRESENTATION_CONTEXT ( 'NONE', 'WORKASPACE' ) );
#418 = ORIENTED_EDGE ( 'NONE', *, *, #1578, .T. ) ;
#419 = ADVANCED_BREP_SHAPE_REPRESENTATION ( '', ( #14292, #6315 ), #9517 ) ;
#420 = CARTESIAN_POINT ( 'NONE',  ( 28.47348575918184110, -58.78531205411836424, -4.199849437517832129 ) ) ;
#421 = AXIS2_PLACEMENT_3D ( 'NONE', #800, #5514, #12747 ) ;
#422 = ORIENTED_EDGE ( 'NONE', *, *, #2866, .F. ) ;
#423 = VECTOR ( 'NONE', #6451, 1000.000000000000000 ) ;
#424 = DIRECTION ( 'NONE',  ( 0.000000000000000000, 0.000000000000000000, -1.000000000000000000 ) ) ;
#425 = DIRECTION ( 'NONE',  ( 0.000000000000000000, -1.000000000000000000, 0.000000000000000000 ) ) ;
#426 = AXIS2_PLACEMENT_3D ( 'NONE', #9506, #14202, #3798 ) ;
#427 = ORIENTED_EDGE ( 'NONE', *, *, #10079, .F. ) ;
#428 = DIRECTION ( 'NONE',  ( 0.000000000000000000, 0.000000000000000000, 1.000000000000000000 ) ) ;
#429 = DIRECTION ( 'NONE',  ( 0.000000000000000000, 0.000000000000000000, 1.000000000000000000 ) ) ;
#430 = ADVANCED_FACE ( 'NONE', ( #12701 ), #5856, .T. ) ;
#431 = EDGE_CURVE ( 'NONE', #7143, #4346, #6, .T. ) ;
#432 = CYLINDRICAL_SURFACE ( 'NONE', #9177, 3.951771890309582869 ) ;
#433 = AXIS2_PLACEMENT_3D ( 'NONE', #3532, #9698, #7289 ) ;
#434 = ORIENTED_EDGE ( 'NONE', *, *, #386, .T. ) ;
#435 = FACE_OUTER_BOUND ( 'NONE', #6645, .T. ) ;
#436 = CONICAL_SURFACE ( 'NONE', #4856, 2.524999999999999467, 0.7853981633973787790 ) ;
#437 = AXIS2_PLACEMENT_3D ( 'NONE', #3487, #8189, #5565 ) ;
#438 = TOROIDAL_SURFACE ( 'NONE', #10274, 12.46463184759105047, 1.000000000000000000 ) ;
#439 = LINE ( 'NONE', #4985, #3268 ) ;
#440 = CARTESIAN_POINT ( 'NONE',  ( 96.29968967959054282, 23.25070940071369208, 33.00000000000012790 ) ) ;
#441 = ORIENTED_EDGE ( 'NONE', *, *, #2442, .F. ) ;
#442 = DIRECTION ( 'NONE',  ( 0.000000000000000000, 0.000000000000000000, 1.000000000000000000 ) ) ;
#443 = ORIENTED_EDGE ( 'NONE', *, *, #5395, .T. ) ;
#444 = CARTESIAN_POINT ( 'NONE',  ( -23.91237149244958360, 3.525053131390499139, 47.66527511103321046 ) ) ;
#445 = AXIS2_PLACEMENT_3D ( 'NONE', #12775, #5776, #7923 ) ;
#446 = VERTEX_POINT ( 'NONE', #13931 ) ;
#447 = CARTESIAN_POINT ( 'NONE',  ( 28.71810018070638648, -65.29678988936899486, 3.348867343503173721 ) ) ;
#448 = ADVANCED_FACE ( 'NONE', ( #7159 ), #15184, .T. ) ;
#449 = EDGE_CURVE ( 'NONE', #4396, #5927, #2469, .T. ) ;
#450 = EDGE_LOOP ( 'NONE', ( #14518, #14522, #9749, #6218 ) ) ;
#451 = AXIS2_PLACEMENT_3D ( 'NONE', #9024, #9337, #11476 ) ;
#452 = CARTESIAN_POINT ( 'NONE',  ( -24.54316048551696028, -7.158540021523408292, 58.00000000000012079 ) ) ;
#453 = LINE ( 'NONE', #3979, #12135 ) ;
#454 = EDGE_LOOP ( 'NONE', ( #9894, #4373, #1618, #2467 ) ) ;
#455 = DIRECTION ( 'NONE',  ( -0.5394184268574523378, 0.8420378618367652113, 0.000000000000000000 ) ) ;
#456 = EDGE_LOOP ( 'NONE', ( #15169, #3093, #13253, #6276 ) ) ;
#457 = CARTESIAN_POINT ( 'NONE',  ( 80.18290120114222930, 29.52935533987996664, -21.00807340887166674 ) ) ;
#458 = LINE ( 'NONE', #7761, #5187 ) ;
#459 = DIRECTION ( 'NONE',  ( -0.5394184268574406804, 0.8420378618367728718, 0.000000000000000000 ) ) ;
#460 = ORIENTED_EDGE ( 'NONE', *, *, #1519, .F. ) ;
#461 = DIRECTION ( 'NONE',  ( -0.000000000000000000, -0.000000000000000000, -1.000000000000000000 ) ) ;
#462 = ORIENTED_EDGE ( 'NONE', *, *, #9510, .T. ) ;
#463 = EDGE_LOOP ( 'NONE', ( #8239, #3179, #633, #6797, #6640 ) ) ;
#464 = DIRECTION ( 'NONE',  ( -0.8208219420614829565, 0.4549890321264266624, 0.3453061251629824246 ) ) ;
#465 = APPLICATION_PROTOCOL_DEFINITION ( 'draft international standard', 'automotive_design', 1998, #14881 ) ;
#466 = ADVANCED_FACE ( 'NONE', ( #3619 ), #3388, .F. ) ;
#467 = DIRECTION ( 'NONE',  ( 0.000000000000000000, 1.000000000000000000, 1.734723475976817547E-15 ) ) ;
#468 =( BOUNDED_SURFACE ( )  B_SPLINE_SURFACE ( 3, 2, ( 
 ( #9739, #10958, #7416 ),
 ( #11029, #14423, #4081 ),
 ( #12112, #6268, #3867 ),
 ( #14564, #12255, #11095 ) ),
 .UNSPECIFIED., .F., .F., .F. ) 
 B_SPLINE_SURFACE_WITH_KNOTS ( ( 4, 4 ),
 ( 3, 3 ),
 ( 0.000000000000000000, 0.001771943201165730557 ),
 ( 0.000000000000000000, 1.000000000000000000 ),
 .UNSPECIFIED. ) 
 GEOMETRIC_REPRESENTATION_ITEM ( )  RATIONAL_B_SPLINE_SURFACE ( (
 ( 1.000000000000000000, 0.8308543624379411963, 1.000000000000000000),
 ( 1.000000000000000000, 0.8288551047899443969, 1.000000000000000000),
 ( 1.000000000000000000, 0.8269348987755755775, 1.000000000000000000),
 ( 1.000000000000000000, 0.8250833044923659987, 1.000000000000000000) ) ) 
 REPRESENTATION_ITEM ( '' )  SURFACE ( )  );
#469 = CARTESIAN_POINT ( 'NONE',  ( -9.657716696386627220, -7.466071317230740689, -47.54143911729025973 ) ) ;
#470 = CARTESIAN_POINT ( 'NONE',  ( 10.05209847106513621, -63.64501252278640919, 2.710939438195351325 ) ) ;
#471 = EDGE_CURVE ( 'NONE', #12214, #14069, #7553, .T. ) ;
#472 = LINE ( 'NONE', #13474, #12021 ) ;
#473 = DIRECTION ( 'NONE',  ( -0.8420378618367644341, -0.5394184268574535590, -0.000000000000000000 ) ) ;
#474 = CARTESIAN_POINT ( 'NONE',  ( 13.86142555056148851, -69.48056866272027321, -4.214447830835809761 ) ) ;
#475 = VECTOR ( 'NONE', #11454, 1000.000000000000000 ) ;
#476 = EDGE_CURVE ( 'NONE', #7436, #10628, #11850, .T. ) ;
#477 = AXIS2_PLACEMENT_3D ( 'NONE', #5498, #9026, #1017 ) ;
#478 = CARTESIAN_POINT ( 'NONE',  ( -9.107478285483566083, 2.086796655788927701, 48.09696226170978406 ) ) ;
#479 = EDGE_LOOP ( 'NONE', ( #6850, #11834, #11522, #3223 ) ) ;
#480 = CARTESIAN_POINT ( 'NONE',  ( 88.00000000000001421, 10.75070940071369208, -33.00000000000012790 ) ) ;
#481 = PLANE ( 'NONE',  #13025 ) ;
#482 = DIRECTION ( 'NONE',  ( 1.000000000000000000, 0.000000000000000000, 0.000000000000000000 ) ) ;
#483 = CARTESIAN_POINT ( 'NONE',  ( 62.00000000000001421, -2.249290599286311032, -38.00000000000012079 ) ) ;
#484 = DIRECTION ( 'NONE',  ( 0.3351302520855081735, 0.000000000000000000, -0.9421718071228324387 ) ) ;
#485 = EDGE_CURVE ( 'NONE', #14513, #11292, #5381, .T. ) ;
#486 = AXIS2_PLACEMENT_3D ( 'NONE', #549, #8705, #618 ) ;
#487 = EDGE_CURVE ( 'NONE', #14705, #9017, #2919, .T. ) ;
#488 = CARTESIAN_POINT ( 'NONE',  ( 47.27423575335444639, 23.25070940071368852, 84.20452624982236500 ) ) ;
#489 = DIRECTION ( 'NONE',  ( -0.000000000000000000, 0.000000000000000000, -1.000000000000000000 ) ) ;
#490 = VERTEX_POINT ( 'NONE', #4780 ) ;
#491 = PLANE ( 'NONE',  #9839 ) ;
#492 = ORIENTED_EDGE ( 'NONE', *, *, #7012, .F. ) ;
#493 = CARTESIAN_POINT ( 'NONE',  ( -25.24562193491511763, -6.954963132161501527, 48.23869654929341522 ) ) ;
#494 = CARTESIAN_POINT ( 'NONE',  ( 80.00000000000001421, -72.24929059928631148, -32.99999999999999289 ) ) ;
#495 = VECTOR ( 'NONE', #4431, 1000.000000000000000 ) ;
#496 = ORIENTED_EDGE ( 'NONE', *, *, #8220, .F. ) ;
#498 = ORIENTED_EDGE ( 'NONE', *, *, #9078, .F. ) ;
#497 = FACE_OUTER_BOUND ( 'NONE', #6933, .T. ) ;
#499 = PLANE ( 'NONE',  #14653 ) ;
#500 = CARTESIAN_POINT ( 'NONE',  ( 29.27360327072251067, -58.32476007869853873, 2.500000000000000000 ) ) ;
#501 = LINE ( 'NONE', #5201, #10269 ) ;
#502 = CARTESIAN_POINT ( 'NONE',  ( 20.86173033120691045, -72.24929059928631148, 3.999999999999999112 ) ) ;
#503 = EDGE_CURVE ( 'NONE', #4611, #7961, #14234, .T. ) ;
#504 = DIRECTION ( 'NONE',  ( -0.000000000000000000, 1.000000000000000000, 1.445602896647339163E-16 ) ) ;
#505 = VERTEX_POINT ( 'NONE', #2771 ) ;
#506 = EDGE_LOOP ( 'NONE', ( #7600, #11130, #5855, #5536 ) ) ;
#507 = CARTESIAN_POINT ( 'NONE',  ( -80.00000000000001421, -74.24929059928631148, 8.000000000000001776 ) ) ;
#508 = AXIS2_PLACEMENT_3D ( 'NONE', #2758, #1819, #6294 ) ;
#509 = ORIENTED_EDGE ( 'NONE', *, *, #3414, .F. ) ;
#510 = DIRECTION ( 'NONE',  ( 1.000000000000000000, 0.000000000000000000, 0.000000000000000000 ) ) ;
#511 = ORIENTED_EDGE ( 'NONE', *, *, #11557, .T. ) ;
#512 = CARTESIAN_POINT ( 'NONE',  ( 27.33509234239454244, -69.49659648540917090, 4.497058153269692937 ) ) ;
#513 = VECTOR ( 'NONE', #15204, 1000.000000000000000 ) ;
#514 = DIRECTION ( 'NONE',  ( 0.000000000000000000, 1.000000000000000000, -0.000000000000000000 ) ) ;
#515 = ORIENTED_EDGE ( 'NONE', *, *, #1099, .T. ) ;
#516 = DIRECTION ( 'NONE',  ( 0.000000000000000000, 0.000000000000000000, -1.000000000000000000 ) ) ;
#517 = DIRECTION ( 'NONE',  ( 0.000000000000000000, 0.000000000000000000, -1.000000000000000000 ) ) ;
#518 = EDGE_LOOP ( 'NONE', ( #85, #11509, #6587, #5049 ) ) ;
#519 = CARTESIAN_POINT ( 'NONE',  ( -80.00000000000001421, -72.24929059928631148, -32.99999999999999289 ) ) ;
#520 = VECTOR ( 'NONE', #3953, 1000.000000000000000 ) ;
#521 = ORIENTED_EDGE ( 'NONE', *, *, #7499, .F. ) ;
#522 = CIRCLE ( 'NONE', #13552, 0.5000000000000004441 ) ;
#523 = FACE_OUTER_BOUND ( 'NONE', #7005, .T. ) ;
#524 = FACE_BOUND ( 'NONE', #11436, .T. ) ;
#525 = EDGE_CURVE ( 'NONE', #14965, #13020, #11921, .T. ) ;
#526 = CARTESIAN_POINT ( 'NONE',  ( 68.02719294894561131, -7.807454411681060691, 82.40005259842790508 ) ) ;
#527 = ORIENTED_EDGE ( 'NONE', *, *, #4321, .T. ) ;
#528 = DIRECTION ( 'NONE',  ( 1.000000000000000000, 0.000000000000000000, 0.000000000000000000 ) ) ;
#529 = ORIENTED_EDGE ( 'NONE', *, *, #4885, .F. ) ;
#530 = AXIS2_PLACEMENT_3D ( 'NONE', #3937, #5033, #8635 ) ;
#531 = VERTEX_POINT ( 'NONE', #1686 ) ;
#532 = VECTOR ( 'NONE', #9239, 1000.000000000000000 ) ;
#533=STYLED_ITEM('',(#15244),#4356);
#534 = CONTEXT_DEPENDENT_SHAPE_REPRESENTATION ( #7513, #14034 ) ;
#535 = FACE_OUTER_BOUND ( 'NONE', #14760, .T. ) ;
#536 = DIRECTION ( 'NONE',  ( -0.9249888031744268879, 0.3799943604870225089, 0.000000000000000000 ) ) ;
#537 = CARTESIAN_POINT ( 'NONE',  ( 114.6731053250840233, 0.000000000000000000, -33.00000000000012790 ) ) ;
#538 = VERTEX_POINT ( 'NONE', #9636 ) ;
#539 = CARTESIAN_POINT ( 'NONE',  ( 64.81656575362153205, -11.48379431191618671, 72.53457481663632223 ) ) ;
#540 = VECTOR ( 'NONE', #9041, 1000.000000000000000 ) ;
#541 = CARTESIAN_POINT ( 'NONE',  ( 114.0000000000000284, 19.25070940071369563, 33.00000000000012790 ) ) ;
#542 = VECTOR ( 'NONE', #2732, 1000.000000000000000 ) ;
#543 = CARTESIAN_POINT ( 'NONE',  ( -16.99999999999998579, -2.249290599286303927, 38.00000000000012079 ) ) ;
#544 = CARTESIAN_POINT ( 'NONE',  ( 10.45251858056743011, -61.76394201830515129, -3.065891788180099553 ) ) ;
#545 = AXIS2_PLACEMENT_3D ( 'NONE', #1167, #6104, #8339 ) ;
#546 = ORIENTED_EDGE ( 'NONE', *, *, #487, .F. ) ;
#547 = CARTESIAN_POINT ( 'NONE',  ( 69.46454297106444642, -2.294433322023684774, 73.19766410831374515 ) ) ;
#548 = CIRCLE ( 'NONE', #9166, 0.5000000000000000000 ) ;
#549 = CARTESIAN_POINT ( 'NONE',  ( -3.190546569013415379, 0.8906624217387615339, 48.50000000000012079 ) ) ;
#550 = VERTEX_POINT ( 'NONE', #9855 ) ;
#551 = SURFACE_STYLE_FILL_AREA ( #9954 ) ;
#552 = DIRECTION ( 'NONE',  ( -0.2245798247307348172, -0.9744556954135535909, 0.000000000000000000 ) ) ;
#553 = AXIS2_PLACEMENT_3D ( 'NONE', #1342, #12818, #9352 ) ;
#554 =( NAMED_UNIT ( * ) PLANE_ANGLE_UNIT ( ) SI_UNIT ( $, .RADIAN. ) );
#555 = CARTESIAN_POINT ( 'NONE',  ( 20.86173033120691045, -74.24929059928636832, -3.999999999999999112 ) ) ;
#556 = VERTEX_POINT ( 'NONE', #13378 ) ;
#557 = CARTESIAN_POINT ( 'NONE',  ( -16.99999999999998579, 2.256146146571129218, 38.00000000000012079 ) ) ;
#558 = AXIS2_PLACEMENT_3D ( 'NONE', #4944, #4869, #3708 ) ;
#559 =( NAMED_UNIT ( * ) SI_UNIT ( $, .STERADIAN. ) SOLID_ANGLE_UNIT ( ) );
#560 = VECTOR ( 'NONE', #4903, 1000.000000000000000 ) ;
#561 = EDGE_CURVE ( 'NONE', #3921, #10500, #8809, .T. ) ;
#562 = DIRECTION ( 'NONE',  ( -0.000000000000000000, -0.000000000000000000, -1.000000000000000000 ) ) ;
#563 = LINE ( 'NONE', #7876, #12055 ) ;
#564 = CARTESIAN_POINT ( 'NONE',  ( 20.86173033120691045, -57.24929059928630437, 0.000000000000000000 ) ) ;
#565 = ORIENTED_EDGE ( 'NONE', *, *, #14825, .T. ) ;
#566 = AXIS2_PLACEMENT_3D ( 'NONE', #4908, #5202, #14225 ) ;
#567 = CARTESIAN_POINT ( 'NONE',  ( 23.50212160826626118, -54.09900330347249309, -6.482993899729486920 ) ) ;
#568 = CIRCLE ( 'NONE', #806, 6.484807146443463566 ) ;
#569 = ORIENTED_EDGE ( 'NONE', *, *, #14553, .F. ) ;
#570 = EDGE_CURVE ( 'NONE', #1671, #7867, #6379, .T. ) ;
#571 = LINE ( 'NONE', #6351, #6668 ) ;
#572 = DIRECTION ( 'NONE',  ( 0.000000000000000000, 0.000000000000000000, -1.000000000000000000 ) ) ;
#573 = ADVANCED_FACE ( 'NONE', ( #1464 ), #315, .F. ) ;
#574 = ORIENTED_EDGE ( 'NONE', *, *, #3154, .F. ) ;
#576 = ORIENTED_EDGE ( 'NONE', *, *, #10446, .T. ) ;
#575 = CARTESIAN_POINT ( 'NONE',  ( 95.31453344691183815, 23.25070940071369208, 33.00000000000012790 ) ) ;
#577 = CARTESIAN_POINT ( 'NONE',  ( 0.000000000000000000, 15.25070940071369563, -13.14990448602693007 ) ) ;
#578 = ORIENTED_EDGE ( 'NONE', *, *, #10333, .T. ) ;
#579 = CARTESIAN_POINT ( 'NONE',  ( 11.75462132594869047, -63.18892729117109042, 3.546101824479054976 ) ) ;
#580 = EDGE_CURVE ( 'NONE', #13749, #4765, #2911, .T. ) ;
#581 = CARTESIAN_POINT ( 'NONE',  ( 11.41483174849314786, -52.33251913750716255, 3.960984348906031460 ) ) ;
#582 = DIRECTION ( 'NONE',  ( 0.000000000000000000, 1.000000000000000000, -0.000000000000000000 ) ) ;
#583 = FACE_OUTER_BOUND ( 'NONE', #10613, .T. ) ;
#584 = ORIENTED_EDGE ( 'NONE', *, *, #12621, .T. ) ;
#585 = FACE_OUTER_BOUND ( 'NONE', #3678, .T. ) ;
#586 = ORIENTED_EDGE ( 'NONE', *, *, #12573, .F. ) ;
#587 = VERTEX_POINT ( 'NONE', #10936 ) ;
#588 = DIRECTION ( 'NONE',  ( -1.000000000000000000, 0.000000000000000000, 0.000000000000000000 ) ) ;
#589 = ORIENTED_EDGE ( 'NONE', *, *, #1386, .T. ) ;
#590 = DIRECTION ( 'NONE',  ( 0.000000000000000000, 0.000000000000000000, 1.000000000000000000 ) ) ;
#591 = DIRECTION ( 'NONE',  ( -1.000000000000000000, 0.000000000000000000, 0.000000000000000000 ) ) ;
#592 = DIRECTION ( 'NONE',  ( 0.000000000000000000, 0.7071067811865965336, 0.7071067811864985009 ) ) ;
#593 = CARTESIAN_POINT ( 'NONE',  ( -9.657716696386627220, -7.466071317230740689, 47.54143911729025973 ) ) ;
#594 = ORIENTED_EDGE ( 'NONE', *, *, #11102, .F. ) ;
#595 = ADVANCED_FACE ( 'NONE', ( #523 ), #13090, .F. ) ;
#596 = DIRECTION ( 'NONE',  ( -9.912705577010325549E-17, 1.734723475976817547E-15, -1.000000000000000000 ) ) ;
#597 = ORIENTED_EDGE ( 'NONE', *, *, #7672, .F. ) ;
#598 = FACE_OUTER_BOUND ( 'NONE', #463, .T. ) ;
#599 = CYLINDRICAL_SURFACE ( 'NONE', #8676, 10.15857703477299623 ) ;
#600 = CARTESIAN_POINT ( 'NONE',  ( 32.39917484285220439, 21.75070940071312364, 33.00000000000012790 ) ) ;
#601 = EDGE_LOOP ( 'NONE', ( #14385, #13165, #13920, #13167 ) ) ;
#602 = LINE ( 'NONE', #8916, #9558 ) ;
#603 = ORIENTED_EDGE ( 'NONE', *, *, #12571, .F. ) ;
#604 = VERTEX_POINT ( 'NONE', #2615 ) ;
#605 = ORIENTED_EDGE ( 'NONE', *, *, #6309, .T. ) ;
#606 = DIRECTION ( 'NONE',  ( -0.000000000000000000, 1.000000000000000000, 1.445602896647339163E-16 ) ) ;
#607 = DIRECTION ( 'NONE',  ( 0.000000000000000000, 0.000000000000000000, 1.000000000000000000 ) ) ;
#608 = PLANE ( 'NONE',  #3506 ) ;
#609 = EDGE_CURVE ( 'NONE', #7436, #1277, #1384, .T. ) ;
#610 = ADVANCED_FACE ( 'NONE', ( #2836 ), #381, .T. ) ;
#611 = CARTESIAN_POINT ( 'NONE',  ( 8.749277640414614865, -56.32592369292856915, -2.799485268159552120 ) ) ;
#612 = VERTEX_POINT ( 'NONE', #13245 ) ;
#613 = LINE ( 'NONE', #1772, #10037 ) ;
#614 = CARTESIAN_POINT ( 'NONE',  ( 61.36510378087922390, 1.530577915148011225, 48.51982618741349285 ) ) ;
#615 = CARTESIAN_POINT ( 'NONE',  ( 14.40311142432127056, -68.64054039872911517, -4.542265185092021262 ) ) ;
#616 = ORIENTED_EDGE ( 'NONE', *, *, #4933, .T. ) ;
#617 = CARTESIAN_POINT ( 'NONE',  ( 33.62912904389242641, -56.86646964060239640, 2.513983171436027231 ) ) ;
#618 = DIRECTION ( 'NONE',  ( 1.000000000000000000, 0.000000000000000000, 0.000000000000000000 ) ) ;
#619 = VERTEX_POINT ( 'NONE', #7390 ) ;
#620 = DIRECTION ( 'NONE',  ( -1.000000000000000000, 0.000000000000000000, 0.000000000000000000 ) ) ;
#621 = FACE_OUTER_BOUND ( 'NONE', #8917, .T. ) ;
#622 = EDGE_CURVE ( 'NONE', #15091, #1508, #10780, .T. ) ;
#623 =( LENGTH_UNIT ( ) NAMED_UNIT ( * ) SI_UNIT ( .MILLI., .METRE. ) );
#624 = CARTESIAN_POINT ( 'NONE',  ( 9.200644618036296407, -59.06479067038043240, -2.757123406423053424 ) ) ;
#625 = VERTEX_POINT ( 'NONE', #1612 ) ;
#626 = CARTESIAN_POINT ( 'NONE',  ( 45.17127246049422240, 21.75070940071322667, 139.1143251403882459 ) ) ;
#627 = CARTESIAN_POINT ( 'NONE',  ( 27.86173033120691045, -69.39711819508848123, -3.801276035476822468 ) ) ;
#628 = CARTESIAN_POINT ( 'NONE',  ( 43.00000000000000711, 15.25070940071368497, 33.00000000000012790 ) ) ;
#629 = DIRECTION ( 'NONE',  ( -0.000000000000000000, 0.000000000000000000, -1.000000000000000000 ) ) ;
#630 = AXIS2_PLACEMENT_3D ( 'NONE', #11136, #591, #8901 ) ;
#631 = ORIENTED_EDGE ( 'NONE', *, *, #11253, .F. ) ;
#632 = CARTESIAN_POINT ( 'NONE',  ( 28.15780090692999593, -63.36830850591302067, -4.156137255743351133 ) ) ;
#633 = ORIENTED_EDGE ( 'NONE', *, *, #14074, .F. ) ;
#634 = DIRECTION ( 'NONE',  ( 0.000000000000000000, -0.000000000000000000, 1.000000000000000000 ) ) ;
#635 = CARTESIAN_POINT ( 'NONE',  ( 58.00000000000000711, -2.249290599286309256, 61.61639468829817190 ) ) ;
#636 = ORIENTED_EDGE ( 'NONE', *, *, #8900, .T. ) ;
#637 = CARTESIAN_POINT ( 'NONE',  ( 0.000000000000000000, 15.25070940071369563, 13.14990448602693007 ) ) ;
#638 = FACE_OUTER_BOUND ( 'NONE', #15061, .T. ) ;
#639 = AXIS2_PLACEMENT_3D ( 'NONE', #12293, #305, #1535 ) ;
#640 = CIRCLE ( 'NONE', #11212, 0.9999999999999996669 ) ;
#641 = EDGE_CURVE ( 'NONE', #13513, #7657, #11510, .T. ) ;
#642 = DIRECTION ( 'NONE',  ( 0.000000000000000000, 0.000000000000000000, 1.000000000000000000 ) ) ;
#643 = CARTESIAN_POINT ( 'NONE',  ( 31.33007899711186894, -52.72918400488543256, -2.651310087704546348 ) ) ;
#644 = AXIS2_PLACEMENT_3D ( 'NONE', #12063, #2755, #14382 ) ;
#645 = EDGE_CURVE ( 'NONE', #11420, #3697, #6168, .T. ) ;
#646 = AXIS2_PLACEMENT_3D ( 'NONE', #2800, #14494, #8783 ) ;
#647 = EDGE_CURVE ( 'NONE', #13534, #13054, #13162, .T. ) ;
#648 = LINE ( 'NONE', #5356, #9186 ) ;
#649 = DIRECTION ( 'NONE',  ( 0.000000000000000000, 0.000000000000000000, -1.000000000000000000 ) ) ;
#650 = ORIENTED_EDGE ( 'NONE', *, *, #10123, .F. ) ;
#651 = AXIS2_PLACEMENT_3D ( 'NONE', #8278, #11802, #11951 ) ;
#652 = DIRECTION ( 'NONE',  ( 0.000000000000000000, 0.000000000000000000, -1.000000000000000000 ) ) ;
#653 = EDGE_LOOP ( 'NONE', ( #6707, #7341, #9588, #14019 ) ) ;
#654 = ADVANCED_FACE ( 'NONE', ( #5008 ), #9713, .F. ) ;
#655 = DIRECTION ( 'NONE',  ( 1.000000000000000000, 0.000000000000000000, 0.000000000000000000 ) ) ;
#656 = EDGE_LOOP ( 'NONE', ( #5765, #14402, #234, #3280, #10430, #12233, #7508, #462, #7848 ) ) ;
#657 = CARTESIAN_POINT ( 'NONE',  ( 64.11356537587559501, -11.94785244090458498, 73.19766410831374515 ) ) ;
#658 = B_SPLINE_CURVE_WITH_KNOTS ( 'NONE', 3,
 ( #10135, #10365, #13747, #3202 ),
 .UNSPECIFIED., .F., .F.,
 ( 4, 4 ),
 ( 0.000000000000000000, 0.001771361151111829372 ),
 .UNSPECIFIED. ) ;
#659 = CARTESIAN_POINT ( 'NONE',  ( 27.55953187330915810, 23.25070940071368852, -33.00000000000012790 ) ) ;
#660 = CARTESIAN_POINT ( 'NONE',  ( 0.000000000000000000, 15.25070940071368497, 139.1143251403882459 ) ) ;
#661 = LINE ( 'NONE', #891, #6723 ) ;
#662 = ORIENTED_EDGE ( 'NONE', *, *, #7032, .T. ) ;
#663 = EDGE_CURVE ( 'NONE', #4371, #14705, #1159, .T. ) ;
#664 = DIRECTION ( 'NONE',  ( 1.000000000000000000, 0.000000000000000000, 0.000000000000000000 ) ) ;
#665 = VECTOR ( 'NONE', #12241, 1000.000000000000000 ) ;
#666 = ORIENTED_EDGE ( 'NONE', *, *, #12524, .F. ) ;
#667 = EDGE_CURVE ( 'NONE', #556, #7206, #3915, .T. ) ;
#668 = CARTESIAN_POINT ( 'NONE',  ( 11.71690433395004227, -52.27452423507673274, -4.068013018868786190 ) ) ;
#669 = DIRECTION ( 'NONE',  ( -0.6198786537240911221, -0.7846976836063734861, 0.000000000000000000 ) ) ;
#670 = CARTESIAN_POINT ( 'NONE',  ( -32.80254285330626374, -2.278009980413908231, 48.50000000000012079 ) ) ;
#671 = CIRCLE ( 'NONE', #2885, 2.524999999999999467 ) ;
#672 = ORIENTED_EDGE ( 'NONE', *, *, #12291, .F. ) ;
#673 = FACE_OUTER_BOUND ( 'NONE', #12478, .T. ) ;
#674 = ORIENTED_EDGE ( 'NONE', *, *, #4052, .T. ) ;
#675 = PRODUCT ( 'Upper Sharpening Angle Guide Base', 'Upper Sharpening Angle Guide Base', '', ( #1396 ) ) ;
#676 = VECTOR ( 'NONE', #14030, 1000.000000000000000 ) ;
#677 = ORIENTED_EDGE ( 'NONE', *, *, #11895, .F. ) ;
#678 = ORIENTED_EDGE ( 'NONE', *, *, #2260, .T. ) ;
#679 = CARTESIAN_POINT ( 'NONE',  ( 58.00000000000000711, -2.249290599286309256, 39.50000000000012790 ) ) ;
#680 = CARTESIAN_POINT ( 'NONE',  ( 8.597635011448854669, -59.20619211347771227, -2.502190571104482952 ) ) ;
#681 = CARTESIAN_POINT ( 'NONE',  ( -24.66543232906180805, 3.122884019241207287, -48.02064173568555816 ) ) ;
#682 = CARTESIAN_POINT ( 'NONE',  ( 54.06723705530823310, -0.06932450177430288241, 87.40005259842790508 ) ) ;
#683 = ORIENTED_EDGE ( 'NONE', *, *, #5858, .F. ) ;
#684 = EDGE_CURVE ( 'NONE', #12779, #2517, #9724, .T. ) ;
#685 = CARTESIAN_POINT ( 'NONE',  ( -80.00000000000001421, -85.24929059928631148, 6.000000000000001776 ) ) ;
#686 = CARTESIAN_POINT ( 'NONE',  ( 18.00000000000001066, 0.000000000000000000, 139.1143251403882459 ) ) ;
#687 = CARTESIAN_POINT ( 'NONE',  ( 0.000000000000000000, 0.000000000000000000, -38.00000000000012079 ) ) ;
#688 = CARTESIAN_POINT ( 'NONE',  ( 12.06814882729969440, -63.62021712492819603, -2.966460067268481549 ) ) ;
#689 = ORIENTED_EDGE ( 'NONE', *, *, #8732, .F. ) ;
#690 = CARTESIAN_POINT ( 'NONE',  ( 69.97972559857382180, -3.172990593254281233, 73.19766410831374515 ) ) ;
#691 = EDGE_CURVE ( 'NONE', #9315, #7200, #11147, .T. ) ;
#692 = ADVANCED_FACE ( 'NONE', ( #8752 ), #5227, .T. ) ;
#693 = CARTESIAN_POINT ( 'NONE',  ( -16.99999999999998579, -2.249290599286303927, -57.50000000000012079 ) ) ;
#694 = ORIENTED_EDGE ( 'NONE', *, *, #1475, .T. ) ;
#695 = CARTESIAN_POINT ( 'NONE',  ( 57.83740799265796539, -7.800393779465814248, 48.51982618741349285 ) ) ;
#696 = CARTESIAN_POINT ( 'NONE',  ( 25.81270058232203013, 21.75070940071309167, -33.00000000000012790 ) ) ;
#697 = CARTESIAN_POINT ( 'NONE',  ( 55.86211336638498182, 2.337731330496643167, 48.51982618741349285 ) ) ;
#698 = DIRECTION ( 'NONE',  ( 0.000000000000000000, -1.000000000000000000, 0.000000000000000000 ) ) ;
#699 = ORIENTED_EDGE ( 'NONE', *, *, #13284, .T. ) ;
#700 = CARTESIAN_POINT ( 'NONE',  ( 8.766252841628377368, -57.08298494442340143, 2.747852995220871009 ) ) ;
#701 = CARTESIAN_POINT ( 'NONE',  ( 10.00023835250150483, -61.42570632716525125, 2.132522520905371977 ) ) ;
#702 = DIRECTION ( 'NONE',  ( 0.8746197071345572782, -0.4848096202550659650, 0.000000000000000000 ) ) ;
#703 = AXIS2_PLACEMENT_3D ( 'NONE', #8419, #1403, #8107 ) ;
#704 = AXIS2_PLACEMENT_3D ( 'NONE', #10886, #8709, #343 ) ;
#705 = CARTESIAN_POINT ( 'NONE',  ( -24.55671735758753726, -7.137878559097176279, -48.23807154671105479 ) ) ;
#706 = EDGE_CURVE ( 'NONE', #7249, #2361, #2636, .T. ) ;
#707 = EDGE_CURVE ( 'NONE', #355, #7994, #45, .T. ) ;
#708 = ORIENTED_EDGE ( 'NONE', *, *, #10704, .T. ) ;
#709 = PLANE ( 'NONE',  #9602 ) ;
#710 = ORIENTED_EDGE ( 'NONE', *, *, #1180, .T. ) ;
#711 = CARTESIAN_POINT ( 'NONE',  ( 55.09646579789918519, -6.394265699299607419, 48.51982618741349285 ) ) ;
#712 = DIRECTION ( 'NONE',  ( 8.659560562354330119E-17, 0.7071067811865966446, -0.7071067811864982788 ) ) ;
#713 = EDGE_LOOP ( 'NONE', ( #4880, #8165, #76, #1992, #12089, #15118, #2455, #11853, #2027, #8217 ) ) ;
#715 = EDGE_LOOP ( 'NONE', ( #1135, #7087, #13779, #14842 ) ) ;
#714 = DIRECTION ( 'NONE',  ( 0.000000000000000000, 0.000000000000000000, 1.000000000000000000 ) ) ;
#716 = CARTESIAN_POINT ( 'NONE',  ( 14.22956937301584546, -69.39711819508849544, -4.416273062436609109 ) ) ;
#717 = ORIENTED_EDGE ( 'NONE', *, *, #12868, .T. ) ;
#718 = AXIS2_PLACEMENT_3D ( 'NONE', #2213, #10452, #821 ) ;
#719 = AXIS2_PLACEMENT_3D ( 'NONE', #5968, #10655, #14038 ) ;
#720 = CARTESIAN_POINT ( 'NONE',  ( 8.649830367478799076, -59.43266865480772054, -1.834006918418332521 ) ) ;
#721 = CARTESIAN_POINT ( 'NONE',  ( 114.0000000000000284, 15.25070940071369563, -13.14990448602693007 ) ) ;
#722 = DIRECTION ( 'NONE',  ( -0.8746197071345572782, 0.4848096202550660205, 0.000000000000000000 ) ) ;
#723 = DIRECTION ( 'NONE',  ( 0.000000000000000000, 0.000000000000000000, 1.000000000000000000 ) ) ;
#724 = CARTESIAN_POINT ( 'NONE',  ( 53.11142512232702018, -3.558169932106523881, 62.84860122826521689 ) ) ;
#725 = AXIS2_PLACEMENT_3D ( 'NONE', #10060, #14667, #13517 ) ;
#726 = ORIENTED_EDGE ( 'NONE', *, *, #9673, .T. ) ;
#727 = EDGE_LOOP ( 'NONE', ( #10150, #492, #10188, #14509 ) ) ;
#728 = DIRECTION ( 'NONE',  ( 0.000000000000000000, 1.000000000000000000, 0.000000000000000000 ) ) ;
#729 = ORIENTED_EDGE ( 'NONE', *, *, #11145, .F. ) ;
#730 = FACE_OUTER_BOUND ( 'NONE', #5305, .T. ) ;
#731 = ORIENTED_EDGE ( 'NONE', *, *, #3102, .F. ) ;
#732 = CARTESIAN_POINT ( 'NONE',  ( 80.00000000000001421, -85.24929059928629727, -8.000000000000001776 ) ) ;
#733 = DIRECTION ( 'NONE',  ( -1.000000000000000000, -0.000000000000000000, -0.000000000000000000 ) ) ;
#734 = CARTESIAN_POINT ( 'NONE',  ( 67.21328690825531282, 25.52935533987996664, -33.00000000000012790 ) ) ;
#735 = CARTESIAN_POINT ( 'NONE',  ( 68.00000000000001421, -2.249290599286293268, 33.00000000000012790 ) ) ;
#736 = ORIENTED_EDGE ( 'NONE', *, *, #1578, .F. ) ;
#737 = EDGE_CURVE ( 'NONE', #9321, #13009, #5442, .T. ) ;
#738 = DIRECTION ( 'NONE',  ( 1.110223024625156540E-15, -1.000000000000000000, 0.000000000000000000 ) ) ;
#739 = ORIENTED_EDGE ( 'NONE', *, *, #13013, .T. ) ;
#740 = EDGE_CURVE ( 'NONE', #6596, #11588, #12572, .T. ) ;
#741 = ADVANCED_FACE ( 'NONE', ( #11639 ), #15109, .F. ) ;
#742 = CARTESIAN_POINT ( 'NONE',  ( 65.13162939602317181, -11.91918766459985157, 75.19766410831374515 ) ) ;
#743 = DIRECTION ( 'NONE',  ( -0.000000000000000000, -0.000000000000000000, -1.000000000000000000 ) ) ;
#744 = CYLINDRICAL_SURFACE ( 'NONE', #11640, 0.4999999999999996669 ) ;
#745 = ORIENTED_EDGE ( 'NONE', *, *, #13734, .T. ) ;
#746 = AXIS2_PLACEMENT_3D ( 'NONE', #2112, #5754, #6809 ) ;
#747 = ORIENTED_EDGE ( 'NONE', *, *, #4471, .F. ) ;
#748 = DIRECTION ( 'NONE',  ( 0.5006040828730401460, -0.8656763553492970997, 0.000000000000000000 ) ) ;
#749 = ORIENTED_EDGE ( 'NONE', *, *, #11198, .T. ) ;
#750 = VERTEX_POINT ( 'NONE', #6949 ) ;
#751 = ADVANCED_FACE ( 'NONE', ( #11790, #1325 ), #12724, .F. ) ;
#752 = CARTESIAN_POINT ( 'NONE',  ( -21.58505662828840599, 4.908031226326156293, -57.50000000000012079 ) ) ;
#753 = EDGE_CURVE ( 'NONE', #12307, #1292, #9416, .T. ) ;
#754 = CIRCLE ( 'NONE', #12822, 0.4999999999999997224 ) ;
#755 = CONTEXT_DEPENDENT_SHAPE_REPRESENTATION ( #3788, #2013 ) ;
#756 = CARTESIAN_POINT ( 'NONE',  ( 52.94134894379979528, -2.395505968190773327, 48.51982618741349285 ) ) ;
#757 = DIRECTION ( 'NONE',  ( -2.775557561562891351E-15, 1.000000000000000000, 0.000000000000000000 ) ) ;
#758 = AXIS2_PLACEMENT_3D ( 'NONE', #11179, #629, #8952 ) ;
#759 = LINE ( 'NONE', #8997, #13503 ) ;
#760 = AXIS2_PLACEMENT_3D ( 'NONE', #3547, #3770, #5009 ) ;
#761 = ORIENTED_EDGE ( 'NONE', *, *, #10485, .F. ) ;
#762 = CARTESIAN_POINT ( 'NONE',  ( 69.99788034154117611, -3.225610097367463514, 75.50178636978743896 ) ) ;
#763 = LINE ( 'NONE', #1921, #4404 ) ;
#764 = CARTESIAN_POINT ( 'NONE',  ( 15.46081644285382772, -69.39711819508849544, 5.076148092048922145 ) ) ;
#765 = DIRECTION ( 'NONE',  ( 0.000000000000000000, -1.000000000000000000, 0.000000000000000000 ) ) ;
#766 = ORIENTED_EDGE ( 'NONE', *, *, #5761, .T. ) ;
#767 = VECTOR ( 'NONE', #133, 1000.000000000000000 ) ;
#768 = CARTESIAN_POINT ( 'NONE',  ( 32.90197589884652274, -57.33450387999031506, 2.749014434309864363 ) ) ;
#769 = TOROIDAL_SURFACE ( 'NONE', #2002, 3.694885682587998765, 0.5000000000000000000 ) ;
#770 = VECTOR ( 'NONE', #9472, 1000.000000000000000 ) ;
#771 = CARTESIAN_POINT ( 'NONE',  ( -20.99999999999998579, -2.249290599286303927, 38.00000000000012079 ) ) ;
#772 = ORIENTED_EDGE ( 'NONE', *, *, #1941, .T. ) ;
#773 = CARTESIAN_POINT ( 'NONE',  ( 29.49975272800921289, -62.74348037527474276, -3.781439773221457301 ) ) ;
#774 = CARTESIAN_POINT ( 'NONE',  ( -29.99999999999998579, -74.24929059928642516, 32.99999999999999289 ) ) ;
#775 = CARTESIAN_POINT ( 'NONE',  ( 52.25109540565180311, -2.012892184189035039, 62.84860122826521689 ) ) ;
#776 = DIRECTION ( 'NONE',  ( 0.000000000000000000, 0.000000000000000000, -1.000000000000000000 ) ) ;
#777 = VERTEX_POINT ( 'NONE', #2331 ) ;
#778 = CARTESIAN_POINT ( 'NONE',  ( 118.0000000000000284, 23.25070940071369563, 139.1143251403882459 ) ) ;
#779 = AXIS2_PLACEMENT_3D ( 'NONE', #15041, #4571, #14877 ) ;
#780 = EDGE_CURVE ( 'NONE', #1026, #927, #5885, .T. ) ;
#781 = AXIS2_PLACEMENT_3D ( 'NONE', #13323, #5092, #9797 ) ;
#782 = CARTESIAN_POINT ( 'NONE',  ( 30.65234355186507997, 21.75070940071312364, 139.1143251403882459 ) ) ;
#783 = CARTESIAN_POINT ( 'NONE',  ( 32.95707784766408110, -57.08357682498795072, 2.747855728348003179 ) ) ;
#784 = VECTOR ( 'NONE', #14829, 1000.000000000000000 ) ;
#785 = CARTESIAN_POINT ( 'NONE',  ( -8.499999999999987566, -2.249290599286303927, -38.00000000000012079 ) ) ;
#786 = CYLINDRICAL_SURFACE ( 'NONE', #758, 0.7892041907098262810 ) ;
#787 = ORIENTED_EDGE ( 'NONE', *, *, #10191, .T. ) ;
#788 = VERTEX_POINT ( 'NONE', #4558 ) ;
#789 = CYLINDRICAL_SURFACE ( 'NONE', #12032, 4.194885682588113340 ) ;
#790 = CIRCLE ( 'NONE', #3744, 2.000000000000000000 ) ;
#791 = VERTEX_POINT ( 'NONE', #9257 ) ;
#792 = CARTESIAN_POINT ( 'NONE',  ( 20.86173033120691045, -57.24929059928630437, 3.000000000000000888 ) ) ;
#793 = DIRECTION ( 'NONE',  ( -0.000000000000000000, 1.000000000000000000, 1.445602896647339163E-16 ) ) ;
#794 = ORIENTED_EDGE ( 'NONE', *, *, #3873, .F. ) ;
#795 = CARTESIAN_POINT ( 'NONE',  ( 56.97758043373130477, 2.707118148285912795, 60.61639468829817190 ) ) ;
#796 = DIRECTION ( 'NONE',  ( -0.000000000000000000, 0.000000000000000000, -1.000000000000000000 ) ) ;
#797 = CIRCLE ( 'NONE', #14087, 1.000000000000001332 ) ;
#798 = CARTESIAN_POINT ( 'NONE',  ( 13.51972775594646947, -66.75404937493283342, 3.551013195535614120 ) ) ;
#799 = ADVANCED_FACE ( 'NONE', ( #1173 ), #14109, .F. ) ;
#800 = CARTESIAN_POINT ( 'NONE',  ( 62.80358567007132820, -3.842053655357405173, 60.61639468829817190 ) ) ;
#801 = CARTESIAN_POINT ( 'NONE',  ( 33.59633122631266389, -57.16466038563396523, -1.814534822646767909 ) ) ;
#802 = FACE_BOUND ( 'NONE', #1169, .T. ) ;
#803 = VECTOR ( 'NONE', #6520, 1000.000000000000000 ) ;
#804 = CARTESIAN_POINT ( 'NONE',  ( 51.75774672102440377, 21.75070940071325865, -33.00000000000012790 ) ) ;
#805 = DIRECTION ( 'NONE',  ( 1.000000000000000000, 0.000000000000000000, 0.000000000000000000 ) ) ;
#806 = AXIS2_PLACEMENT_3D ( 'NONE', #12943, #2078, #13935 ) ;
#807 = ORIENTED_EDGE ( 'NONE', *, *, #6638, .F. ) ;
#808 = CARTESIAN_POINT ( 'NONE',  ( 7.497055383622185154, -51.17811635675307969, -2.733205671937324777 ) ) ;
#809 = ORIENTED_EDGE ( 'NONE', *, *, #5886, .F. ) ;
#810 = LINE ( 'NONE', #13901, #15019 ) ;
#811 = ORIENTED_EDGE ( 'NONE', *, *, #7029, .T. ) ;
#812 = CARTESIAN_POINT ( 'NONE',  ( 103.2469880950108063, 23.25070940071369208, -33.00000000000012790 ) ) ;
#813 = LINE ( 'NONE', #2986, #1383 ) ;
#814 = ADVANCED_FACE ( 'NONE', ( #10570 ), #5184, .T. ) ;
#815 = CARTESIAN_POINT ( 'NONE',  ( 46.91810375148135392, 23.25070940071368852, 33.00000000000012790 ) ) ;
#816 = DIRECTION ( 'NONE',  ( 0.000000000000000000, 0.000000000000000000, -1.000000000000000000 ) ) ;
#817 = ORIENTED_EDGE ( 'NONE', *, *, #5665, .F. ) ;
#818 = VECTOR ( 'NONE', #7680, 1000.000000000000000 ) ;
#819 = FACE_OUTER_BOUND ( 'NONE', #7730, .T. ) ;
#820 = EDGE_LOOP ( 'NONE', ( #5722, #8057, #10459, #9791, #8309 ) ) ;
#821 = DIRECTION ( 'NONE',  ( 1.000000000000000000, 0.000000000000000000, 0.000000000000000000 ) ) ;
#822 = CARTESIAN_POINT ( 'NONE',  ( 8.605785544313173219, -54.47948885957401188, -2.876625435111462625 ) ) ;
#823 = CARTESIAN_POINT ( 'NONE',  ( 80.18290120114222930, 25.52935533987996664, 84.20452624982236500 ) ) ;
#824 = DIRECTION ( 'NONE',  ( 1.000000000000000000, 0.000000000000000000, 0.000000000000000000 ) ) ;
#825 = ORIENTED_EDGE ( 'NONE', *, *, #1492, .T. ) ;
#826 = ORIENTED_EDGE ( 'NONE', *, *, #11805, .F. ) ;
#827 = CARTESIAN_POINT ( 'NONE',  ( 80.18290120114222930, 29.52935533987996664, 21.00807340887166674 ) ) ;
#828 = ADVANCED_FACE ( 'NONE', ( #11712 ), #13872, .T. ) ;
#829 = EDGE_LOOP ( 'NONE', ( #10229, #6980, #7558, #1341 ) ) ;
#830 = CARTESIAN_POINT ( 'NONE',  ( 100.0000000000000284, 11.25070940071369563, -33.00000000000012790 ) ) ;
#831 = ORIENTED_EDGE ( 'NONE', *, *, #11996, .T. ) ;
#832 = EDGE_LOOP ( 'NONE', ( #908, #9068, #8291, #12526 ) ) ;
#833 = CARTESIAN_POINT ( 'NONE',  ( 121.4079758241357609, -32.82348926221179397, 57.22220354671984666 ) ) ;
#834 = FACE_OUTER_BOUND ( 'NONE', #12615, .T. ) ;
#835 = CARTESIAN_POINT ( 'NONE',  ( 10.21509949969620834, -53.84182990103197142, -3.477143273224481579 ) ) ;
#836 = FACE_OUTER_BOUND ( 'NONE', #10102, .T. ) ;
#837 = ADVANCED_FACE ( 'NONE', ( #8103 ), #14260, .F. ) ;
#838 = ORIENTED_EDGE ( 'NONE', *, *, #12621, .F. ) ;
#839 = DIRECTION ( 'NONE',  ( -0.000000000000000000, 0.000000000000000000, 1.000000000000000000 ) ) ;
#840 = CARTESIAN_POINT ( 'NONE',  ( 32.90197589884652274, -57.33450387999030085, -2.749014434309871024 ) ) ;
#841 = ADVANCED_FACE ( 'NONE', ( #12100 ), #14411, .F. ) ;
#842 = DIRECTION ( 'NONE',  ( -0.000000000000000000, -0.000000000000000000, -1.000000000000000000 ) ) ;
#843 = ADVANCED_FACE ( 'NONE', ( #8557 ), #10988, .F. ) ;
#844 = VERTEX_POINT ( 'NONE', #5167 ) ;
#845 = ADVANCED_FACE ( 'NONE', ( #1698 ), #6393, .F. ) ;
#846 = CARTESIAN_POINT ( 'NONE',  ( 69.45807991563580686, -2.948854807202607731, 72.84297311730249191 ) ) ;
#847 = LINE ( 'NONE', #1850, #4677 ) ;
#848 = ORIENTED_EDGE ( 'NONE', *, *, #10704, .F. ) ;
#849 = CARTESIAN_POINT ( 'NONE',  ( 27.69711443911335991, -66.46764508687284945, -4.441229594909795964 ) ) ;
#850 = DIRECTION ( 'NONE',  ( 1.000000000000000000, 1.156482317317870492E-16, 0.000000000000000000 ) ) ;
#851 = ADVANCED_FACE ( 'NONE', ( #9652 ), #14341, .F. ) ;
#852 = ORIENTED_EDGE ( 'NONE', *, *, #5942, .T. ) ;
#853 = B_SPLINE_CURVE_WITH_KNOTS ( 'NONE', 3,
 ( #870, #3338, #5576, #8037, #7337, #2342 ),
 .UNSPECIFIED., .F., .F.,
 ( 4, 2, 4 ),
 ( 0.000000000000000000, 0.008081365602589977992, 0.01616273120517995598 ),
 .UNSPECIFIED. ) ;
#854 =( LENGTH_UNIT ( ) NAMED_UNIT ( * ) SI_UNIT ( .MILLI., .METRE. ) );
#855 = LINE ( 'NONE', #14787, #8320 ) ;
#856 = DIRECTION ( 'NONE',  ( 0.000000000000000000, -1.000000000000000000, 0.000000000000000000 ) ) ;
#857 = APPLICATION_CONTEXT ( 'automotive_design' ) ;
#858 = ORIENTED_EDGE ( 'NONE', *, *, #14035, .T. ) ;
#859 = FACE_OUTER_BOUND ( 'NONE', #13100, .T. ) ;
#860 = DIRECTION ( 'NONE',  ( 0.9839406800755990945, -0.1784957649143745217, 0.000000000000000000 ) ) ;
#861 = DIRECTION ( 'NONE',  ( -0.000000000000000000, 0.000000000000000000, -1.000000000000000000 ) ) ;
#862 = FACE_OUTER_BOUND ( 'NONE', #2285, .T. ) ;
#863 = CARTESIAN_POINT ( 'NONE',  ( 67.21328690825529861, 29.52935533987996664, -21.00807340887166674 ) ) ;
#864 = VERTEX_POINT ( 'NONE', #12532 ) ;
#865 = ORIENTED_EDGE ( 'NONE', *, *, #8044, .F. ) ;
#866 = VECTOR ( 'NONE', #2481, 1000.000000000000000 ) ;
#867 = CARTESIAN_POINT ( 'NONE',  ( 27.90872427450967663, -67.42803803071015523, -4.083598241683256802 ) ) ;
#868 = ORIENTED_EDGE ( 'NONE', *, *, #13611, .F. ) ;
#869 = CARTESIAN_POINT ( 'NONE',  ( 30.65234355186507997, 23.25070940071368852, 33.00000000000012790 ) ) ;
#870 = CARTESIAN_POINT ( 'NONE',  ( 24.10826840236108737, -69.39711819508849544, 6.201611931792130328 ) ) ;
#871 = ORIENTED_EDGE ( 'NONE', *, *, #15074, .F. ) ;
#872 = DIRECTION ( 'NONE',  ( 0.000000000000000000, 0.000000000000000000, -1.000000000000000000 ) ) ;
#873 = CARTESIAN_POINT ( 'NONE',  ( 116.1386546156546444, -40.19284343218672007, 54.40673322733725570 ) ) ;
#874 = AXIS2_PLACEMENT_3D ( 'NONE', #14984, #10447, #6820 ) ;
#875 = LINE ( 'NONE', #15126, #9021 ) ;
#876 = CARTESIAN_POINT ( 'NONE',  ( 30.90164406145839138, -52.52607756353321378, -2.773424542755355660 ) ) ;
#877 = DIRECTION ( 'NONE',  ( 1.000000000000000000, 0.000000000000000000, 0.000000000000000000 ) ) ;
#878 = CARTESIAN_POINT ( 'NONE',  ( 82.49066175147797253, 12.46743062497963450, -33.00000000000012790 ) ) ;
#879 = VERTEX_POINT ( 'NONE', #7688 ) ;
#880 = CARTESIAN_POINT ( 'NONE',  ( 17.58146340911262584, -70.03159917003323187, -6.184016381205385215 ) ) ;
#881 = EDGE_CURVE ( 'NONE', #5130, #10222, #5376, .T. ) ;
#882 = EDGE_CURVE ( 'NONE', #9663, #7432, #3526, .T. ) ;
#883 = ORIENTED_EDGE ( 'NONE', *, *, #13767, .T. ) ;
#884 = CARTESIAN_POINT ( 'NONE',  ( 8.201103799357262858, -57.48563641131178770, 1.816685854991387794 ) ) ;
#885 = CIRCLE ( 'NONE', #12695, 0.7892041907098275022 ) ;
#886 = ORIENTED_EDGE ( 'NONE', *, *, #4268, .T. ) ;
#887 = CARTESIAN_POINT ( 'NONE',  ( -16.99999999999998579, -2.249290599286303927, -58.00000000000012079 ) ) ;
#888 = CIRCLE ( 'NONE', #9509, 0.4999999999999997780 ) ;
#889 = DIRECTION ( 'NONE',  ( 0.000000000000000000, 0.000000000000000000, 1.000000000000000000 ) ) ;
#890 = CARTESIAN_POINT ( 'NONE',  ( -8.537170960192302260, 2.067018546614596719, -48.00000000000012079 ) ) ;
#891 = CARTESIAN_POINT ( 'NONE',  ( -2.016677571526633510E-15, 23.25070940071368497, 33.00000000000012790 ) ) ;
#892 = AXIS2_PLACEMENT_3D ( 'NONE', #6524, #1690, #528 ) ;
#893 = CARTESIAN_POINT ( 'NONE',  ( 65.00000000000001421, -87.24929059928631148, -19.99999999999999645 ) ) ;
#894 = ORIENTED_EDGE ( 'NONE', *, *, #4866, .T. ) ;
#895 = VECTOR ( 'NONE', #2862, 1000.000000000000000 ) ;
#896 = DIRECTION ( 'NONE',  ( 1.000000000000000000, 0.000000000000000000, 0.000000000000000000 ) ) ;
#897 = CARTESIAN_POINT ( 'NONE',  ( 8.615075654522891924, -54.46933172536110845, -2.097670533079140309 ) ) ;
#898 = DIRECTION ( 'NONE',  ( 1.000000000000000000, 0.000000000000000000, 0.000000000000000000 ) ) ;
#899 = FACE_OUTER_BOUND ( 'NONE', #4695, .T. ) ;
#900 = ORIENTED_EDGE ( 'NONE', *, *, #4035, .F. ) ;
#901 = EDGE_CURVE ( 'NONE', #298, #3805, #11869, .T. ) ;
#902 = EDGE_CURVE ( 'NONE', #251, #11798, #9174, .T. ) ;
#903 = CARTESIAN_POINT ( 'NONE',  ( -7.499999999999985789, -2.249290599286303927, 47.50000000000012079 ) ) ;
#904 = VECTOR ( 'NONE', #10762, 1000.000000000000114 ) ;
#905 = PRODUCT_DEFINITION ( 'UNKNOWN', '', #1171, #3354 ) ;
#906 = EDGE_LOOP ( 'NONE', ( #132, #13235, #5815, #2969 ) ) ;
#907 = CARTESIAN_POINT ( 'NONE',  ( -26.99999999999998934, -2.249290599286303927, 38.00000000000012079 ) ) ;
#908 = ORIENTED_EDGE ( 'NONE', *, *, #2368, .F. ) ;
#909 = AXIS2_PLACEMENT_3D ( 'NONE', #991, #9316, #8085 ) ;
#910 = VECTOR ( 'NONE', #6269, 999.9999999999998863 ) ;
#911 = CARTESIAN_POINT ( 'NONE',  ( 9.654882263607307280, -61.15288932781407283, -2.038807541293268688 ) ) ;
#912 = CARTESIAN_POINT ( 'NONE',  ( -21.85476584171706449, 5.329050157244580532, -48.50000000000012079 ) ) ;
#913 = CARTESIAN_POINT ( 'NONE',  ( 11.08356997321305393, -53.42334933900650640, -3.800563870772192043 ) ) ;
#914 = CARTESIAN_POINT ( 'NONE',  ( 109.8334623555409735, 0.000000000000000000, 13.14990448602693007 ) ) ;
#915 = EDGE_LOOP ( 'NONE', ( #9268, #4270, #12205, #3537 ) ) ;
#916 = VECTOR ( 'NONE', #1039, 1000.000000000000000 ) ;
#917 = CARTESIAN_POINT ( 'NONE',  ( 65.00000000000001421, -85.24929059928629727, -19.99999999999999645 ) ) ;
#918 = CARTESIAN_POINT ( 'NONE',  ( 33.63443549450521175, -56.24768769701492488, -2.562823873651032258 ) ) ;
#919 = CARTESIAN_POINT ( 'NONE',  ( 27.60269520869854887, -53.27034158699149913, 4.884662653952318578 ) ) ;
#920 = CARTESIAN_POINT ( 'NONE',  ( 32.22669677403312960, -60.90158242457943771, 2.720958399978099074 ) ) ;
#921 = VECTOR ( 'NONE', #8754, 1000.000000000000000 ) ;
#922 = VERTEX_POINT ( 'NONE', #11287 ) ;
#923 = VECTOR ( 'NONE', #12640, 1000.000000000000000 ) ;
#924 = CARTESIAN_POINT ( 'NONE',  ( 69.28051765693513175, -4.295678830383772961, 72.19766410831373094 ) ) ;
#925 = DIRECTION ( 'NONE',  ( 0.000000000000000000, 1.000000000000000000, 0.000000000000000000 ) ) ;
#926 = ADVANCED_FACE ( 'NONE', ( #10219 ), #599, .F. ) ;
#927 = VERTEX_POINT ( 'NONE', #5454 ) ;
#928 = AXIS2_PLACEMENT_3D ( 'NONE', #14541, #7614, #1981 ) ;
#929 = SHAPE_REPRESENTATION_RELATIONSHIP ( 'NONE' , 'NONE' ,  #2449, #8343 ) ;
#930 = CARTESIAN_POINT ( 'NONE',  ( 112.9262740340969060, 0.000000000000000000, 139.1143251403882459 ) ) ;
#931 = VERTEX_POINT ( 'NONE', #8912 ) ;
#932 = VECTOR ( 'NONE', #5247, 1000.000000000000000 ) ;
#933 = CARTESIAN_POINT ( 'NONE',  ( -8.787473000605775297, 2.499856724880853864, -48.43453164808066447 ) ) ;
#934 = CARTESIAN_POINT ( 'NONE',  ( -33.07225206673494711, -1.856991049495498425, -48.50000000000012079 ) ) ;
#935 = CARTESIAN_POINT ( 'NONE',  ( 80.00000000000001421, -74.24929059928631148, -4.000000000000000000 ) ) ;
#936 = DIRECTION ( 'NONE',  ( 0.8420378618367728718, 0.5394184268574404584, 0.000000000000000000 ) ) ;
#937 = EDGE_CURVE ( 'NONE', #7143, #11623, #10072, .T. ) ;
#938 = CARTESIAN_POINT ( 'NONE',  ( -65.00000000000001421, -85.24929059928629727, -19.99999999999999645 ) ) ;
#939 = ORIENTED_EDGE ( 'NONE', *, *, #13244, .T. ) ;
#940 = ORIENTED_EDGE ( 'NONE', *, *, #12365, .F. ) ;
#941 = CARTESIAN_POINT ( 'NONE',  ( 0.000000000000000000, 21.75070940071325865, 139.1143251403882459 ) ) ;
#942 = VECTOR ( 'NONE', #14321, 1000.000000000000000 ) ;
#943 = VERTEX_POINT ( 'NONE', #12611 ) ;
#944 = CARTESIAN_POINT ( 'NONE',  ( -28.70947653109703523, -9.020656969121422009, -57.50000000000012079 ) ) ;
#945 = CARTESIAN_POINT ( 'NONE',  ( 11.00552470667372340, -52.46278122153624679, 2.824859710458689666 ) ) ;
#946 = ORIENTED_EDGE ( 'NONE', *, *, #10645, .T. ) ;
#947 = CARTESIAN_POINT ( 'NONE',  ( 60.05137561479872232, 2.911430354694811484, 48.51982618741349285 ) ) ;
#948 = DIRECTION ( 'NONE',  ( -0.000000000000000000, 0.000000000000000000, -1.000000000000000000 ) ) ;
#949 = EDGE_CURVE ( 'NONE', #3754, #3249, #2996, .T. ) ;
#950 = EDGE_CURVE ( 'NONE', #9272, #7803, #4209, .T. ) ;
#951 = LINE ( 'NONE', #6885, #9647 ) ;
#952 = AXIS2_PLACEMENT_3D ( 'NONE', #10166, #3233, #14775 ) ;
#953 =( BOUNDED_SURFACE ( )  B_SPLINE_SURFACE ( 3, 2, ( 
 ( #11003, #4136, #12769 ),
 ( #2218, #2299, #5613 ),
 ( #975, #5847, #11363 ),
 ( #7840, #12685, #2137 ),
 ( #3216, #9227, #15146 ),
 ( #15078, #3141, #6830 ),
 ( #14908, #3450, #10455 ),
 ( #8147, #10379, #10303 ) ),
 .UNSPECIFIED., .F., .F., .F. ) 
 B_SPLINE_SURFACE_WITH_KNOTS ( ( 4, 2, 2, 4 ),
 ( 3, 3 ),
 ( -6.505213034913026604E-19, 0.001129222206655588513, 0.002258444413311177894, 0.004516888826622356655 ),
 ( 0.000000000000000000, 1.000000000000000000 ),
 .UNSPECIFIED. ) 
 GEOMETRIC_REPRESENTATION_ITEM ( )  RATIONAL_B_SPLINE_SURFACE ( (
 ( 1.000000000000000000, 0.7071067811864926167, 1.000000000000000000),
 ( 1.000000000000000000, 0.7608707698419998611, 1.000000000000000000),
 ( 1.000000000000000000, 0.8047257278452493168, 1.000000000000000000),
 ( 1.000000000000000000, 0.8783509392183369568, 1.000000000000000000),
 ( 1.000000000000000000, 0.9081758943107525184, 1.000000000000000000),
 ( 1.000000000000000000, 0.9781389570701306546, 1.000000000000000000),
 ( 1.000000000000000000, 0.9996704379322433054, 1.000000000000000000),
 ( 1.000000000000000000, 1.000000000000000000, 1.000000000000000000) ) ) 
 REPRESENTATION_ITEM ( '' )  SURFACE ( )  );
#954 = DIRECTION ( 'NONE',  ( 0.8420378618367644341, 0.5394184268574535590, 0.000000000000000000 ) ) ;
#955 = CARTESIAN_POINT ( 'NONE',  ( 31.49298359385885959, -60.71197230342421136, 3.050751728647414840 ) ) ;
#956 = CARTESIAN_POINT ( 'NONE',  ( 0.6601805061683232445, -1.030548743169294346, 57.50000000000012079 ) ) ;
#957 = CARTESIAN_POINT ( 'NONE',  ( 40.33162949095117966, 23.25070940071368852, -33.00000000000012790 ) ) ;
#958 = DIRECTION ( 'NONE',  ( -9.912705577010325549E-17, 1.734723475976817547E-15, -1.000000000000000000 ) ) ;
#959 = ORIENTED_EDGE ( 'NONE', *, *, #13649, .F. ) ;
#960 = CYLINDRICAL_SURFACE ( 'NONE', #11471, 2.499999999999995115 ) ;
#961 = ORIENTED_EDGE ( 'NONE', *, *, #6671, .T. ) ;
#962 = AXIS2_PLACEMENT_3D ( 'NONE', #12322, #765, #7710 ) ;
#963 = CARTESIAN_POINT ( 'NONE',  ( 62.00000000000001421, -2.249290599286310588, 33.00000000000012790 ) ) ;
#964 = AXIS2_PLACEMENT_3D ( 'NONE', #11793, #936, #4486 ) ;
#965 = VERTEX_POINT ( 'NONE', #11361 ) ;
#966 = LINE ( 'NONE', #2988, #12194 ) ;
#967 = LINE ( 'NONE', #2211, #12353 ) ;
#968 = ORIENTED_EDGE ( 'NONE', *, *, #5858, .T. ) ;
#969 = EDGE_CURVE ( 'NONE', #12642, #2618, #1832, .T. ) ;
#970 = AXIS2_PLACEMENT_3D ( 'NONE', #941, #13800, #11326 ) ;
#971 = FACE_OUTER_BOUND ( 'NONE', #5210, .T. ) ;
#972 = CARTESIAN_POINT ( 'NONE',  ( 10.86432672294017365, -53.50034303113530143, -3.720434809418780908 ) ) ;
#973 = DIRECTION ( 'NONE',  ( 1.000000000000000000, 1.156482317317870492E-16, 0.000000000000000000 ) ) ;
#974 = EDGE_CURVE ( 'NONE', #11391, #10817, #14814, .T. ) ;
#975 = CARTESIAN_POINT ( 'NONE',  ( -9.657039156986668260, -7.465117833064532249, 47.54128347411995037 ) ) ;
#976 = ORIENTED_EDGE ( 'NONE', *, *, #9709, .T. ) ;
#977 = VERTEX_POINT ( 'NONE', #14993 ) ;
#978 = DIRECTION ( 'NONE',  ( 0.3020115420618247892, -0.1674077314120183957, 0.9384901064608620613 ) ) ;
#979 = ORIENTED_EDGE ( 'NONE', *, *, #14140, .T. ) ;
#980 = CARTESIAN_POINT ( 'NONE',  ( -2.688903428702175252E-15, 23.25070940071368142, 33.00000000000012790 ) ) ;
#981 = VERTEX_POINT ( 'NONE', #6749 ) ;
#982 = AXIS2_PLACEMENT_3D ( 'NONE', #8563, #2856, #340 ) ;
#983 = DIRECTION ( 'NONE',  ( -0.4848096202550659650, -0.8746197071345572782, 0.000000000000000000 ) ) ;
#984 = DIRECTION ( 'NONE',  ( 0.000000000000000000, 0.000000000000000000, 1.000000000000000000 ) ) ;
#985 = CARTESIAN_POINT ( 'NONE',  ( 54.00000000000000711, -2.249290599286310588, -49.31370849898490150 ) ) ;
#986 = CYLINDRICAL_SURFACE ( 'NONE', #5207, 4.665819364273509073 ) ;
#987 = EDGE_CURVE ( 'NONE', #7237, #11741, #11214, .T. ) ;
#988 = ORIENTED_EDGE ( 'NONE', *, *, #12071, .F. ) ;
#989 = ADVANCED_FACE ( 'NONE', ( #7762 ), #6601, .F. ) ;
#990 = VECTOR ( 'NONE', #350, 1000.000000000000000 ) ;
#991 = CARTESIAN_POINT ( 'NONE',  ( 58.00000000000000711, -2.249290599286311032, 38.50000000000012790 ) ) ;
#992 = CARTESIAN_POINT ( 'NONE',  ( 0.000000000000000000, 21.75070940071309167, 139.1143251403882459 ) ) ;
#993 = CARTESIAN_POINT ( 'NONE',  ( 69.41637355099324225, -3.305665566658139376, 76.92699484961572409 ) ) ;
#994 = DIRECTION ( 'NONE',  ( -0.000000000000000000, -0.000000000000000000, -1.000000000000000000 ) ) ;
#995 = DIRECTION ( 'NONE',  ( -1.000000000000000000, -0.000000000000000000, -0.000000000000000000 ) ) ;
#996 = VERTEX_POINT ( 'NONE', #9154 ) ;
#997 = CARTESIAN_POINT ( 'NONE',  ( 17.09549820959326638, -85.24929059928631148, 1.347403282660979640 ) ) ;
#998 = CARTESIAN_POINT ( 'NONE',  ( 18.24487436548682240, -53.24929059928630437, 6.492462156583975741 ) ) ;
#999 = AXIS2_PLACEMENT_3D ( 'NONE', #14231, #1449, #6157 ) ;
#1000 = EDGE_LOOP ( 'NONE', ( #9467, #6469, #14232, #3569 ) ) ;
#1001 = DIRECTION ( 'NONE',  ( 1.000000000000000000, 0.000000000000000000, 0.000000000000000000 ) ) ;
#1002 = SURFACE_STYLE_FILL_AREA ( #6857 ) ;
#1003 = ORIENTED_EDGE ( 'NONE', *, *, #8126, .F. ) ;
#1004=STYLED_ITEM('',(#15279),#4097);
#1005 = AXIS2_PLACEMENT_3D ( 'NONE', #15165, #10318, #12789 ) ;
#1006 = ORIENTED_EDGE ( 'NONE', *, *, #15185, .F. ) ;
#1007 = DIRECTION ( 'NONE',  ( -0.000000000000000000, -0.000000000000000000, -1.000000000000000000 ) ) ;
#1008 = FACE_OUTER_BOUND ( 'NONE', #715, .T. ) ;
#1009 = EDGE_LOOP ( 'NONE', ( #9822, #6669, #1334, #10838 ) ) ;
#1010 = EDGE_CURVE ( 'NONE', #879, #9712, #9431, .T. ) ;
#1011 = CARTESIAN_POINT ( 'NONE',  ( -12.99999999999998757, -2.249290599286303483, 36.00000000000012079 ) ) ;
#1012 = DIRECTION ( 'NONE',  ( -0.000000000000000000, 0.000000000000000000, 1.000000000000000000 ) ) ;
#1013 = VECTOR ( 'NONE', #13265, 1000.000000000000000 ) ;
#1014 = PLANE ( 'NONE',  #7092 ) ;
#1015 = CARTESIAN_POINT ( 'NONE',  ( 31.88839645113984034, -54.14139889408636463, 3.328424545751987651 ) ) ;
#1016 = CIRCLE ( 'NONE', #2502, 5.496540510819668768 ) ;
#1017 = DIRECTION ( 'NONE',  ( 0.3020115420618323387, -0.1674077314120217264, 0.9384901064608589527 ) ) ;
#1018 = LINE ( 'NONE', #2095, #4193 ) ;
#1019 = VECTOR ( 'NONE', #8713, 1000.000000000000000 ) ;
#1020 = ORIENTED_EDGE ( 'NONE', *, *, #14571, .F. ) ;
#1021 = ORIENTED_EDGE ( 'NONE', *, *, #8257, .F. ) ;
#1022 = CARTESIAN_POINT ( 'NONE',  ( -24.96222495693456978, -7.431276100536581275, -48.50000000000012079 ) ) ;
#1023 = ORIENTED_EDGE ( 'NONE', *, *, #15171, .T. ) ;
#1024 = DIRECTION ( 'NONE',  ( 0.1784957649143733838, 0.9839406800755994276, -0.000000000000000000 ) ) ;
#1025 = CARTESIAN_POINT ( 'NONE',  ( 8.233817939642571915, -55.39655954610098121, 1.945404611338338974 ) ) ;
#1026 = VERTEX_POINT ( 'NONE', #8983 ) ;
#1027 = VECTOR ( 'NONE', #1162, 1000.000000000000000 ) ;
#1028 = PLANE ( 'NONE',  #14565 ) ;
#1029 = DIRECTION ( 'NONE',  ( 0.000000000000000000, -1.000000000000000000, 1.927470528863120035E-16 ) ) ;
#1030 = AXIS2_PLACEMENT_3D ( 'NONE', #11882, #5895, #6042 ) ;
#1031 = EDGE_CURVE ( 'NONE', #922, #3003, #2788, .T. ) ;
#1032 = CIRCLE ( 'NONE', #3494, 1.000000000000000000 ) ;
#1033 = DIRECTION ( 'NONE',  ( 0.8746197071345573892, -0.4848096202550657430, 0.000000000000000000 ) ) ;
#1034 = CARTESIAN_POINT ( 'NONE',  ( 20.86173033120691045, -52.24929059928630437, 0.000000000000000000 ) ) ;
#1035 = LINE ( 'NONE', #2428, #12248 ) ;
#1036 = CARTESIAN_POINT ( 'NONE',  ( 20.86173033120691045, -72.24929059928631148, -7.000000000000000000 ) ) ;
#1037 = CARTESIAN_POINT ( 'NONE',  ( 27.55953187330915810, 21.75070940071309167, 139.1143251403882459 ) ) ;
#1038 = VECTOR ( 'NONE', #8723, 1000.000000000000000 ) ;
#1039 = DIRECTION ( 'NONE',  ( -1.000000000000000000, -1.156482317317870492E-16, 0.000000000000000000 ) ) ;
#1040 = EDGE_CURVE ( 'NONE', #12282, #6181, #9065, .T. ) ;
#1041 = VECTOR ( 'NONE', #698, 1000.000000000000000 ) ;
#1042 = ORIENTED_EDGE ( 'NONE', *, *, #3581, .T. ) ;
#1043 = EDGE_CURVE ( 'NONE', #604, #5327, #4004, .T. ) ;
#1044 = CARTESIAN_POINT ( 'NONE',  ( 9.843069943267799715, -62.60658208063265562, -2.715520055324554427 ) ) ;
#1045 = UNCERTAINTY_MEASURE_WITH_UNIT (LENGTH_MEASURE( 1.000000000000000082E-05 ), #9181, 'distance_accuracy_value', 'NONE');
#1046 = VECTOR ( 'NONE', #9005, 1000.000000000000000 ) ;
#1047 = ORIENTED_EDGE ( 'NONE', *, *, #11121, .T. ) ;
#1048 = LINE ( 'NONE', #210, #4481 ) ;
#1049 = ORIENTED_EDGE ( 'NONE', *, *, #13035, .F. ) ;
#1050 = CARTESIAN_POINT ( 'NONE',  ( 1.004339113574583608, 0.8906624217387615339, 48.00000000000012079 ) ) ;
#1051 = CARTESIAN_POINT ( 'NONE',  ( 68.02719294894561131, -7.807454411681058026, 81.40005259842790508 ) ) ;
#1052 = DIRECTION ( 'NONE',  ( 0.000000000000000000, 0.000000000000000000, 1.000000000000000000 ) ) ;
#1053 = ADVANCED_FACE ( 'NONE', ( #1060 ), #68, .F. ) ;
#1054 = CARTESIAN_POINT ( 'NONE',  ( 45.17127246049422240, 21.75070940071322667, 33.00000000000012790 ) ) ;
#1055 = AXIS2_PLACEMENT_3D ( 'NONE', #3787, #9729, #7919 ) ;
#1056 = ORIENTED_EDGE ( 'NONE', *, *, #10977, .T. ) ;
#1057 = VECTOR ( 'NONE', #994, 1000.000000000000000 ) ;
#1058 = DIRECTION ( 'NONE',  ( -0.000000000000000000, -1.000000000000000000, 4.625929269271485914E-16 ) ) ;
#1059 = CARTESIAN_POINT ( 'NONE',  ( 10.02953924049373313, -52.92218391219020646, -3.457912412237230892 ) ) ;
#1060 = FACE_OUTER_BOUND ( 'NONE', #4938, .T. ) ;
#1061 = CARTESIAN_POINT ( 'NONE',  ( 20.86173033120691045, -72.24929059928631148, -3.999999999999999112 ) ) ;
#1062 = ORIENTED_EDGE ( 'NONE', *, *, #6313, .F. ) ;
#1063 = CARTESIAN_POINT ( 'NONE',  ( 33.25707175992483400, -58.63671300496854144, 1.826958383950116671 ) ) ;
#1064 = ORIENTED_EDGE ( 'NONE', *, *, #11189, .T. ) ;
#1065 = DIRECTION ( 'NONE',  ( 0.000000000000000000, 0.000000000000000000, 1.000000000000000000 ) ) ;
#1066 = ORIENTED_EDGE ( 'NONE', *, *, #11069, .F. ) ;
#1067 = CIRCLE ( 'NONE', #10913, 0.7892041907098261699 ) ;
#1068 = EDGE_CURVE ( 'NONE', #2182, #12939, #10900, .T. ) ;
#1069 = VECTOR ( 'NONE', #4442, 1000.000000000000000 ) ;
#1070 = EDGE_LOOP ( 'NONE', ( #1164, #3149 ) ) ;
#1071 = PLANE ( 'NONE',  #4829 ) ;
#1072 = DIRECTION ( 'NONE',  ( -0.000000000000000000, 0.000000000000000000, -1.000000000000000000 ) ) ;
#1073 = LINE ( 'NONE', #10467, #9643 ) ;
#1074 = DIRECTION ( 'NONE',  ( 0.000000000000000000, 1.000000000000000000, -0.000000000000000000 ) ) ;
#1075 = ORIENTED_EDGE ( 'NONE', *, *, #10722, .F. ) ;
#1076 = LINE ( 'NONE', #3311, #11234 ) ;
#1077 = CARTESIAN_POINT ( 'NONE',  ( 64.65840159946851884, -11.60091655178341696, 72.83455400280563197 ) ) ;
#1078 = DIRECTION ( 'NONE',  ( 0.3020115420618247892, -0.1674077314120183957, 0.9384901064608620613 ) ) ;
#1079 = DIRECTION ( 'NONE',  ( 0.000000000000000000, 0.000000000000000000, 1.000000000000000000 ) ) ;
#1080 = ORIENTED_EDGE ( 'NONE', *, *, #1195, .F. ) ;
#1081 = DIRECTION ( 'NONE',  ( -0.000000000000000000, -0.000000000000000000, -1.000000000000000000 ) ) ;
#1082 = ADVANCED_FACE ( 'NONE', ( #8143 ), #6990, .T. ) ;
#1083 = VERTEX_POINT ( 'NONE', #14148 ) ;
#1084 = EDGE_CURVE ( 'NONE', #4458, #166, #5687, .T. ) ;
#1085 = DIRECTION ( 'NONE',  ( -0.000000000000000000, -0.000000000000000000, -1.000000000000000000 ) ) ;
#1086 = DIRECTION ( 'NONE',  ( 1.000000000000000000, 0.000000000000000000, 0.000000000000000000 ) ) ;
#1087 = DIRECTION ( 'NONE',  ( 0.000000000000000000, 0.000000000000000000, 1.000000000000000000 ) ) ;
#1088 = CARTESIAN_POINT ( 'NONE',  ( 56.56161818778031858, -7.613266777470379942, 54.56811043785582882 ) ) ;
#1089 = VERTEX_POINT ( 'NONE', #3597 ) ;
#1090 = LINE ( 'NONE', #3173, #14166 ) ;
#1091 = CARTESIAN_POINT ( 'NONE',  ( -2.688903428702175252E-15, 23.25070940071368142, 139.1143251403882459 ) ) ;
#1092 = CARTESIAN_POINT ( 'NONE',  ( 8.700857908379099115, -59.65407802634350531, 1.835581805806634215 ) ) ;
#1093 = CARTESIAN_POINT ( 'NONE',  ( 54.30726695196912601, -6.397170215889376621, 60.61639468829817190 ) ) ;
#1094 = CARTESIAN_POINT ( 'NONE',  ( 52.72873328492558187, -0.5014548242779776066, 54.56811043785582882 ) ) ;
#1095 = CARTESIAN_POINT ( 'NONE',  ( -80.00000000000001421, -74.24929059928631148, 32.99999999999999289 ) ) ;
#1096 = VERTEX_POINT ( 'NONE', #9302 ) ;
#1097 = ADVANCED_FACE ( 'NONE', ( #8307 ), #11826, .F. ) ;
#1098 = FACE_OUTER_BOUND ( 'NONE', #13950, .T. ) ;
#1099 = EDGE_CURVE ( 'NONE', #3217, #9619, #12876, .T. ) ;
#1100 = ORIENTED_EDGE ( 'NONE', *, *, #561, .F. ) ;
#1101 = LINE ( 'NONE', #5813, #11583 ) ;
#1102 = CARTESIAN_POINT ( 'NONE',  ( 32.05792886619255455, -60.12744825561602369, -2.859530283892876668 ) ) ;
#1103 = ORIENTED_EDGE ( 'NONE', *, *, #3765, .F. ) ;
#1104 = DIRECTION ( 'NONE',  ( 0.000000000000000000, 1.000000000000000000, 0.000000000000000000 ) ) ;
#1105 = CARTESIAN_POINT ( 'NONE',  ( 23.47858629692699139, -53.24929059928630437, 6.492462156583989064 ) ) ;
#1106 = DIRECTION ( 'NONE',  ( -0.000000000000000000, 1.000000000000000000, 0.000000000000000000 ) ) ;
#1107 = CARTESIAN_POINT ( 'NONE',  ( 24.62796245282055452, -96.56299909827106376, -1.347403282660978752 ) ) ;
#1108 = DIRECTION ( 'NONE',  ( 1.000000000000000000, 0.000000000000000000, 0.000000000000000000 ) ) ;
#1109 = CARTESIAN_POINT ( 'NONE',  ( 24.62796245282055452, -85.24929059928631148, 1.347403282660977641 ) ) ;
#1110 = LINE ( 'NONE', #2350, #5012 ) ;
#1111 = VERTEX_POINT ( 'NONE', #2446 ) ;
#1112 = CARTESIAN_POINT ( 'NONE',  ( 12.65255919500326165, -50.97757525706221315, -4.214488946479060694 ) ) ;
#1113 = EDGE_LOOP ( 'NONE', ( #12679, #6087, #3200, #7335 ) ) ;
#1114 = CARTESIAN_POINT ( 'NONE',  ( -16.99999999999998579, -2.249290599286303927, 36.00000000000012079 ) ) ;
#1115 = VERTEX_POINT ( 'NONE', #10454 ) ;
#1116 = CARTESIAN_POINT ( 'NONE',  ( 14.03037318137822886, -66.48338622332325087, -4.442552071294021410 ) ) ;
#1117 = VERTEX_POINT ( 'NONE', #9537 ) ;
#1118 = FACE_OUTER_BOUND ( 'NONE', #3433, .T. ) ;
#1119 = EDGE_CURVE ( 'NONE', #1157, #384, #4495, .T. ) ;
#1120 = DIRECTION ( 'NONE',  ( -1.000000000000000000, 0.000000000000000000, 0.000000000000000000 ) ) ;
#1121 = VECTOR ( 'NONE', #11160, 1000.000000000000000 ) ;
#1122 = DIRECTION ( 'NONE',  ( 1.000000000000000000, 0.000000000000000000, 0.000000000000000000 ) ) ;
#1123 = EDGE_CURVE ( 'NONE', #5327, #943, #11624, .T. ) ;
#1124 = EDGE_CURVE ( 'NONE', #11720, #12161, #8919, .T. ) ;
#1125 = VERTEX_POINT ( 'NONE', #10604 ) ;
#1126 = DIRECTION ( 'NONE',  ( 0.000000000000000000, 0.000000000000000000, 1.000000000000000000 ) ) ;
#1127 = CARTESIAN_POINT ( 'NONE',  ( 50.01091543003727224, 0.000000000000000000, -33.00000000000012790 ) ) ;
#1128 = DIRECTION ( 'NONE',  ( 0.8746197071345569451, -0.4848096202550666312, 0.000000000000000000 ) ) ;
#1129 = CYLINDRICAL_SURFACE ( 'NONE', #6973, 1.000000000000000444 ) ;
#1130 = EDGE_CURVE ( 'NONE', #10151, #9216, #11372, .T. ) ;
#1131 = EDGE_CURVE ( 'NONE', #7651, #2922, #2136, .T. ) ;
#1132 = ORIENTED_EDGE ( 'NONE', *, *, #2690, .T. ) ;
#1133 = VECTOR ( 'NONE', #7599, 1000.000000000000000 ) ;
#1134 = FACE_OUTER_BOUND ( 'NONE', #14394, .T. ) ;
#1135 = ORIENTED_EDGE ( 'NONE', *, *, #12418, .T. ) ;
#1136 = PLANE ( 'NONE',  #5436 ) ;
#1137 = ORIENTED_EDGE ( 'NONE', *, *, #10778, .F. ) ;
#1138 = EDGE_LOOP ( 'NONE', ( #6793, #4822, #4988, #10304 ) ) ;
#1139 = EDGE_CURVE ( 'NONE', #4676, #7142, #8068, .T. ) ;
#1140 = CARTESIAN_POINT ( 'NONE',  ( 54.17164678268019173, 2.103670757168142114, 60.61639468829817190 ) ) ;
#1141 = DIRECTION ( 'NONE',  ( -0.000000000000000000, -1.000000000000000000, -1.734723475976817547E-15 ) ) ;
#1142 = ORIENTED_EDGE ( 'NONE', *, *, #4718, .F. ) ;
#1143 = EDGE_CURVE ( 'NONE', #6567, #14796, #12851, .T. ) ;
#1144 = AXIS2_PLACEMENT_3D ( 'NONE', #660, #5528, #12372 ) ;
#1145 = ADVANCED_FACE ( 'NONE', ( #4680 ), #2298, .T. ) ;
#1146 = DIRECTION ( 'NONE',  ( 1.000000000000000000, -0.000000000000000000, -0.000000000000000000 ) ) ;
#1147 = AXIS2_PLACEMENT_3D ( 'NONE', #7440, #3671, #285 ) ;
#1148 = CARTESIAN_POINT ( 'NONE',  ( 88.00000000000000000, 23.25070940071369208, -33.00000000000012790 ) ) ;
#1149 = ORIENTED_EDGE ( 'NONE', *, *, #11411, .F. ) ;
#1150 = DIRECTION ( 'NONE',  ( 1.734723475976807292E-15, -1.000000000000000000, 0.000000000000000000 ) ) ;
#1151 = CARTESIAN_POINT ( 'NONE',  ( 54.00000000000000711, -2.249290599286311032, 33.00000000000012790 ) ) ;
#1152 = AXIS2_PLACEMENT_3D ( 'NONE', #12756, #4427, #9132 ) ;
#1153 = ADVANCED_FACE ( 'NONE', ( #11515 ), #2215, .F. ) ;
#1154 = DIRECTION ( 'NONE',  ( -0.8746197071345569451, 0.4848096202550666312, 0.000000000000000000 ) ) ;
#1155 = CARTESIAN_POINT ( 'NONE',  ( 27.90816809802827692, -67.42878071151913844, 4.083908651743608509 ) ) ;
#1156 = AXIS2_PLACEMENT_3D ( 'NONE', #7171, #2325, #5725 ) ;
#1157 = VERTEX_POINT ( 'NONE', #6907 ) ;
#1158 = DIRECTION ( 'NONE',  ( -1.110223024625156540E-15, 1.000000000000000000, 0.000000000000000000 ) ) ;
#1159 = CIRCLE ( 'NONE', #5842, 0.5000000000000008882 ) ;
#1160 = VECTOR ( 'NONE', #10730, 1000.000000000000000 ) ;
#1161 = ORIENTED_EDGE ( 'NONE', *, *, #780, .F. ) ;
#1162 = DIRECTION ( 'NONE',  ( 1.051347561198064835E-16, 0.000000000000000000, 1.000000000000000000 ) ) ;
#1163 = CARTESIAN_POINT ( 'NONE',  ( 18.61871093201826355, -53.24929059928630437, 5.564967562786272914 ) ) ;
#1164 = ORIENTED_EDGE ( 'NONE', *, *, #7456, .T. ) ;
#1165 = CARTESIAN_POINT ( 'NONE',  ( 0.000000000000000000, 0.000000000000000000, 0.000000000000000000 ) ) ;
#1166 = PLANE ( 'NONE',  #9038 ) ;
#1167 = CARTESIAN_POINT ( 'NONE',  ( -32.80254285330622110, -2.278009980413880697, 48.50000000000012079 ) ) ;
#1168 = ORIENTED_EDGE ( 'NONE', *, *, #11677, .T. ) ;
#1169 = EDGE_LOOP ( 'NONE', ( #1100, #441 ) ) ;
#1170 = CIRCLE ( 'NONE', #6821, 9.500000000000001776 ) ;
#1171 = PRODUCT_DEFINITION_FORMATION_WITH_SPECIFIED_SOURCE ( 'ANY', '', #1909, .NOT_KNOWN. ) ;
#1172 = FACE_OUTER_BOUND ( 'NONE', #2030, .T. ) ;
#1173 = FACE_OUTER_BOUND ( 'NONE', #9518, .T. ) ;
#1174 = AXIS2_PLACEMENT_3D ( 'NONE', #11340, #12661, #954 ) ;
#1175 = EDGE_CURVE ( 'NONE', #10461, #3922, #7367, .T. ) ;
#1176 = VECTOR ( 'NONE', #14022, 1000.000000000000000 ) ;
#1177 = EDGE_CURVE ( 'NONE', #9470, #12642, #1669, .T. ) ;
#1178 = FACE_OUTER_BOUND ( 'NONE', #3126, .T. ) ;
#1179 = DIRECTION ( 'NONE',  ( -0.000000000000000000, 0.000000000000000000, -1.000000000000000000 ) ) ;
#1180 = EDGE_CURVE ( 'NONE', #11520, #11986, #1561, .T. ) ;
#1181 = CARTESIAN_POINT ( 'NONE',  ( 20.86173033120691045, -87.24929059928631148, 0.000000000000000000 ) ) ;
#1182 = DIRECTION ( 'NONE',  ( 0.000000000000000000, 0.000000000000000000, 1.000000000000000000 ) ) ;
#1183 = CIRCLE ( 'NONE', #7088, 2.499999999999995115 ) ;
#1184 = VERTEX_POINT ( 'NONE', #1443 ) ;
#1185 = DIRECTION ( 'NONE',  ( -0.000000000000000000, -0.000000000000000000, -1.000000000000000000 ) ) ;
#1186 = EDGE_LOOP ( 'NONE', ( #7240, #3544 ) ) ;
#1187 = CARTESIAN_POINT ( 'NONE',  ( -8.842479278987921631, -7.118053859731281463, -48.00000000000012079 ) ) ;
#1188 = CARTESIAN_POINT ( 'NONE',  ( 18.16985775135671943, -55.94205978621073427, 6.462225911923643373 ) ) ;
#1189 = VECTOR ( 'NONE', #10286, 1000.000000000000000 ) ;
#1190 = EDGE_LOOP ( 'NONE', ( #8131, #3911, #5540, #4860 ) ) ;
#1191 = CARTESIAN_POINT ( 'NONE',  ( 71.15942379059755751, -15.26044865788734484, 71.19766410831374515 ) ) ;
#1192 = DIRECTION ( 'NONE',  ( 0.000000000000000000, 0.000000000000000000, 1.000000000000000000 ) ) ;
#1193 = CARTESIAN_POINT ( 'NONE',  ( 13.86584091103555139, -68.67486713609712012, 3.656664647209427521 ) ) ;
#1194 = EDGE_CURVE ( 'NONE', #9216, #11968, #7461, .T. ) ;
#1195 = EDGE_CURVE ( 'NONE', #10628, #10836, #7216, .T. ) ;
#1196 = DIRECTION ( 'NONE',  ( -0.000000000000000000, -0.000000000000000000, 1.000000000000000000 ) ) ;
#1197 = CARTESIAN_POINT ( 'NONE',  ( -16.99999999999998579, -2.249290599286303927, 50.00000000000012079 ) ) ;
#1198 = CARTESIAN_POINT ( 'NONE',  ( -25.46282903980763024, -6.565599745187293834, 48.00000000000012079 ) ) ;
#1199 = PRODUCT_DEFINITION ( 'UNKNOWN', '', #11005, #4748 ) ;
#1200 = CARTESIAN_POINT ( 'NONE',  ( 13.86173033120691223, -69.39711819508849544, 3.619682905202618262 ) ) ;
#1201 = CARTESIAN_POINT ( 'NONE',  ( 32.13751574144283296, -54.40403913628106380, 3.226152465599038344 ) ) ;
#1202 = DIRECTION ( 'NONE',  ( 1.000000000000000000, 3.647594591642515023E-31, -2.102695122396130409E-16 ) ) ;
#1203 = ORIENTED_EDGE ( 'NONE', *, *, #14249, .T. ) ;
#1204 = DIRECTION ( 'NONE',  ( 0.5454721580263366398, -0.8381289428352246551, 4.385647630081457888E-16 ) ) ;
#1205 = ORIENTED_EDGE ( 'NONE', *, *, #6548, .T. ) ;
#1206 = ORIENTED_EDGE ( 'NONE', *, *, #9236, .T. ) ;
#1207 = CARTESIAN_POINT ( 'NONE',  ( 65.18141112804345028, -11.90723896596971798, 75.46703592544538708 ) ) ;
#1208 = CARTESIAN_POINT ( 'NONE',  ( 21.74884261173415467, -96.56299909827106376, -4.000000000000000888 ) ) ;
#1209 = LINE ( 'NONE', #4592, #1781 ) ;
#1210 = ORIENTED_EDGE ( 'NONE', *, *, #3031, .T. ) ;
#1211 = CARTESIAN_POINT ( 'NONE',  ( -6.999999999999987566, -2.249290599286300818, -115.4621125123531442 ) ) ;
#1212 = CARTESIAN_POINT ( 'NONE',  ( -16.99999999999998579, -67.96969602390581144, -115.4621125123531442 ) ) ;
#1213 = AXIS2_PLACEMENT_3D ( 'NONE', #5888, #13034, #4946 ) ;
#1214 = CIRCLE ( 'NONE', #477, 0.9999999999999948930 ) ;
#1215 = ORIENTED_EDGE ( 'NONE', *, *, #949, .F. ) ;
#1216 = ORIENTED_EDGE ( 'NONE', *, *, #4415, .T. ) ;
#1217 = CARTESIAN_POINT ( 'NONE',  ( 65.32299310458444097, -11.07130256205453200, 77.13099622499589714 ) ) ;
#1218 = ORIENTED_EDGE ( 'NONE', *, *, #5311, .F. ) ;
#1219 = CARTESIAN_POINT ( 'NONE',  ( 4.848008884920353090, 21.49656883983473676, 0.000000000000000000 ) ) ;
#1220 = EDGE_LOOP ( 'NONE', ( #9030, #9222, #106, #3497 ) ) ;
#1221 = ORIENTED_EDGE ( 'NONE', *, *, #8483, .F. ) ;
#1222 = EDGE_CURVE ( 'NONE', #20, #13907, #11903, .T. ) ;
#1223 = CARTESIAN_POINT ( 'NONE',  ( -23.91237149244958360, 3.525053131390499139, -47.66527511103321046 ) ) ;
#1224 = CARTESIAN_POINT ( 'NONE',  ( -30.00000000000000000, 23.95881716715930665, -32.99999999999982236 ) ) ;
#1225 = EDGE_LOOP ( 'NONE', ( #8488, #1205, #7597, #4474 ) ) ;
#1226 = EDGE_CURVE ( 'NONE', #5867, #10383, #2818, .T. ) ;
#1227 = TOROIDAL_SURFACE ( 'NONE', #6624, 10.46463184759104870, 1.000000000000000000 ) ;
#1228 = FACE_OUTER_BOUND ( 'NONE', #1806, .T. ) ;
#1229 = CARTESIAN_POINT ( 'NONE',  ( 69.97972559857382180, -3.172990593254279457, 73.19766410831374515 ) ) ;
#1230 = ORIENTED_EDGE ( 'NONE', *, *, #9692, .T. ) ;
#1231 = DIRECTION ( 'NONE',  ( 1.000000000000000000, 0.000000000000000000, 0.000000000000000000 ) ) ;
#1232 = LINE ( 'NONE', #382, #3479 ) ;
#1233 = CARTESIAN_POINT ( 'NONE',  ( 47.97280705105441001, 3.308873213108444400, 61.61639468829817190 ) ) ;
#1234 = ORIENTED_EDGE ( 'NONE', *, *, #15073, .T. ) ;
#1235 = CARTESIAN_POINT ( 'NONE',  ( 69.41342053903602505, -3.337090261597983609, 71.45041864562929845 ) ) ;
#1236 = EDGE_CURVE ( 'NONE', #11968, #14491, #439, .T. ) ;
#1237 = EDGE_CURVE ( 'NONE', #11933, #12860, #5235, .T. ) ;
#1238 = ORIENTED_EDGE ( 'NONE', *, *, #9123, .F. ) ;
#1239 = DIRECTION ( 'NONE',  ( -1.110223024625156540E-15, 1.000000000000000000, 0.000000000000000000 ) ) ;
#1240 = DIRECTION ( 'NONE',  ( 0.8746197071345569451, -0.4848096202550666312, 0.000000000000000000 ) ) ;
#1241 = EDGE_LOOP ( 'NONE', ( #9052, #8384, #14542, #4784 ) ) ;
#1242 = CARTESIAN_POINT ( 'NONE',  ( 0.000000000000000000, 0.000000000000000000, 0.000000000000000000 ) ) ;
#1243 = CARTESIAN_POINT ( 'NONE',  ( 61.57572300660984865, -8.804762498903286883, 75.19766410831374515 ) ) ;
#1244 = DIRECTION ( 'NONE',  ( 0.000000000000000000, 0.000000000000000000, 1.000000000000000000 ) ) ;
#1245 = ORIENTED_EDGE ( 'NONE', *, *, #645, .F. ) ;
#1246 = DIRECTION ( 'NONE',  ( 0.000000000000000000, 0.000000000000000000, 1.000000000000000000 ) ) ;
#1247 = CARTESIAN_POINT ( 'NONE',  ( 32.87486430914729141, -60.00492685494704403, -2.531405393170241158 ) ) ;
#1248 = PLANE ( 'NONE',  #2409 ) ;
#1249 = CARTESIAN_POINT ( 'NONE',  ( 28.08719811482655970, -65.28118056119629387, 4.304032224033948140 ) ) ;
#1250 = CARTESIAN_POINT ( 'NONE',  ( 14.46725369622999402, -52.24929059928630437, -3.946667064627067845 ) ) ;
#1251 = CARTESIAN_POINT ( 'NONE',  ( 31.16509434949074731, -52.62744651407953000, -3.653242136006408014 ) ) ;
#1252 = AXIS2_PLACEMENT_3D ( 'NONE', #11270, #13666, #13822 ) ;
#1253 = EDGE_LOOP ( 'NONE', ( #1021, #5256, #6232, #324 ) ) ;
#1254 = VECTOR ( 'NONE', #14887, 1000.000000000000000 ) ;
#1255 = DIRECTION ( 'NONE',  ( -0.8746197071345555019, 0.4848096202550691847, 0.000000000000000000 ) ) ;
#1256 = ORIENTED_EDGE ( 'NONE', *, *, #1813, .F. ) ;
#1257 = DIRECTION ( 'NONE',  ( 0.000000000000000000, 0.000000000000000000, 1.000000000000000000 ) ) ;
#1258 = CARTESIAN_POINT ( 'NONE',  ( 17.87818865416385705, -64.01730164816845559, 6.333338579777398891 ) ) ;
#1259 = FACE_OUTER_BOUND ( 'NONE', #10043, .T. ) ;
#1260 = LINE ( 'NONE', #5974, #11225 ) ;
#1261 = ADVANCED_FACE ( 'NONE', ( #9762 ), #6148, .T. ) ;
#1262 = CARTESIAN_POINT ( 'NONE',  ( -1.243300532054838308E-15, 10.75070940071368142, -33.00000000000012790 ) ) ;
#1263 = VECTOR ( 'NONE', #5764, 1000.000000000000000 ) ;
#1264 = FILL_AREA_STYLE ('',( #10664 ) ) ;
#1265 = EDGE_LOOP ( 'NONE', ( #4395, #8035, #13913, #9464 ) ) ;
#1266 = AXIS2_PLACEMENT_3D ( 'NONE', #2022, #489, #12411 ) ;
#1267 = DIRECTION ( 'NONE',  ( 0.8746197071345570562, -0.4848096202550665756, 0.000000000000000000 ) ) ;
#1268 = CARTESIAN_POINT ( 'NONE',  ( -25.43628086306388525, -6.625164433253370788, 48.00000000000012079 ) ) ;
#1269 = PLANE ( 'NONE',  #7327 ) ;
#1270 = CARTESIAN_POINT ( 'NONE',  ( 33.43717902155964339, -55.20947656326173103, 1.969991847668780993 ) ) ;
#1271 = CARTESIAN_POINT ( 'NONE',  ( 80.00000000000001421, -85.24929059928629727, 32.00000000000000000 ) ) ;
#1272 = VECTOR ( 'NONE', #1085, 1000.000000000000000 ) ;
#1273 = AXIS2_PLACEMENT_3D ( 'NONE', #8800, #13496, #6352 ) ;
#1274 = ORIENTED_EDGE ( 'NONE', *, *, #4240, .F. ) ;
#1275 = LINE ( 'NONE', #10675, #767 ) ;
#1276 = AXIS2_PLACEMENT_3D ( 'NONE', #9205, #12823, #13888 ) ;
#1277 = VERTEX_POINT ( 'NONE', #3964 ) ;
#1278 = DIRECTION ( 'NONE',  ( -0.000000000000000000, 1.000000000000000000, -0.000000000000000000 ) ) ;
#1279 = PLANE ( 'NONE',  #11718 ) ;
#1280 = ADVANCED_FACE ( 'NONE', ( #8522, #10758 ), #218, .T. ) ;
#1281 = CARTESIAN_POINT ( 'NONE',  ( 72.42321995572909543, -14.81762824354790276, 76.19766410831374515 ) ) ;
#1282 = AXIS2_PLACEMENT_3D ( 'NONE', #2665, #5347, #6422 ) ;
#1283 = CARTESIAN_POINT ( 'NONE',  ( 9.670226323787769473, -54.31204422905957330, 3.261005077968429422 ) ) ;
#1284 = VECTOR ( 'NONE', #12777, 1000.000000000000000 ) ;
#1285 = VECTOR ( 'NONE', #3850, 1000.000000000000000 ) ;
#1286 = DIRECTION ( 'NONE',  ( 0.000000000000000000, -1.000000000000000000, 0.000000000000000000 ) ) ;
#1287 = DIRECTION ( 'NONE',  ( 0.8746197071345572782, -0.4848096202550659650, 0.000000000000000000 ) ) ;
#1288 = AXIS2_PLACEMENT_3D ( 'NONE', #12935, #13082, #1377 ) ;
#1289 = EDGE_LOOP ( 'NONE', ( #2796, #13787, #11153, #13533, #11758, #578, #321, #745 ) ) ;
#1290 = EDGE_LOOP ( 'NONE', ( #3521, #15102, #569, #10478, #1685 ) ) ;
#1291 = DIRECTION ( 'NONE',  ( 0.000000000000000000, 0.000000000000000000, -1.000000000000000000 ) ) ;
#1292 = VERTEX_POINT ( 'NONE', #502 ) ;
#1293 = DIRECTION ( 'NONE',  ( 0.000000000000000000, 0.000000000000000000, 1.000000000000000000 ) ) ;
#1294 = ORIENTED_EDGE ( 'NONE', *, *, #2324, .T. ) ;
#1295 = FACE_OUTER_BOUND ( 'NONE', #8669, .T. ) ;
#1296 = EDGE_CURVE ( 'NONE', #3181, #6626, #5246, .T. ) ;
#1297 = VECTOR ( 'NONE', #3657, 1000.000000000000000 ) ;
#1298 = ORIENTED_EDGE ( 'NONE', *, *, #8807, .T. ) ;
#1299 = VECTOR ( 'NONE', #2746, 1000.000000000000000 ) ;
#1300 = CARTESIAN_POINT ( 'NONE',  ( -2.688903428702175252E-15, 23.25070940071368142, 33.00000000000012790 ) ) ;
#1301 = FACE_OUTER_BOUND ( 'NONE', #10786, .T. ) ;
#1302 = ORIENTED_EDGE ( 'NONE', *, *, #11228, .F. ) ;
#1303 = VECTOR ( 'NONE', #9531, 1000.000000000000000 ) ;
#1304 = CARTESIAN_POINT ( 'NONE',  ( -24.12409601409935078, -6.885803942510236197, -57.50000000000012079 ) ) ;
#1305 = DIRECTION ( 'NONE',  ( 0.000000000000000000, 0.000000000000000000, -1.000000000000000000 ) ) ;
#1306 = ORIENTED_EDGE ( 'NONE', *, *, #10977, .F. ) ;
#1307 = CARTESIAN_POINT ( 'NONE',  ( -30.80945343098651890, -5.389243620311580329, -48.00000000000012079 ) ) ;
#1308 = DIRECTION ( 'NONE',  ( -0.000000000000000000, -0.000000000000000000, -1.000000000000000000 ) ) ;
#1309 = EDGE_CURVE ( 'NONE', #12008, #14442, #8458, .T. ) ;
#1310 = DIRECTION ( 'NONE',  ( -0.8656763553492639041, -0.5006040828730973224, 0.000000000000000000 ) ) ;
#1311 = VERTEX_POINT ( 'NONE', #9697 ) ;
#1312 = VECTOR ( 'NONE', #7448, 1000.000000000000000 ) ;
#1313 = CARTESIAN_POINT ( 'NONE',  ( 65.13162939602315760, -11.91918766459984980, 73.04333912804901274 ) ) ;
#1314 = AXIS2_PLACEMENT_3D ( 'NONE', #6602, #11288, #7612 ) ;
#1315 = ORIENTED_EDGE ( 'NONE', *, *, #6502, .T. ) ;
#1316 = FACE_OUTER_BOUND ( 'NONE', #2115, .T. ) ;
#1317 = CARTESIAN_POINT ( 'NONE',  ( -3.190546569013415379, 0.8906624217387615339, 48.50000000000012079 ) ) ;
#1318 = ORIENTED_EDGE ( 'NONE', *, *, #5485, .T. ) ;
#1319 = SHAPE_REPRESENTATION_RELATIONSHIP ( 'NONE' , 'NONE' ,  #11972, #8677 ) ;
#1320 = CARTESIAN_POINT ( 'NONE',  ( -28.70947653109703168, -9.020656969121420232, 48.00000000000012079 ) ) ;
#1321 = EDGE_CURVE ( 'NONE', #7274, #6176, #11638, .T. ) ;
#1322 = CARTESIAN_POINT ( 'NONE',  ( 121.1059642820739128, -32.65608153079976006, 56.28371344025897827 ) ) ;
#1323 = ORIENTED_EDGE ( 'NONE', *, *, #13700, .F. ) ;
#1324 = LINE ( 'NONE', #11711, #12676 ) ;
#1325 = FACE_BOUND ( 'NONE', #10555, .T. ) ;
#1326 = EDGE_CURVE ( 'NONE', #7147, #298, #13221, .T. ) ;
#1327 = AXIS2_PLACEMENT_3D ( 'NONE', #8905, #1894, #6592 ) ;
#1328 = EDGE_CURVE ( 'NONE', #505, #1125, #2947, .T. ) ;
#1329 = ADVANCED_FACE ( 'NONE', ( #5059 ), #3895, .F. ) ;
#1330 = DIRECTION ( 'NONE',  ( -1.000000000000000000, -0.000000000000000000, -0.000000000000000000 ) ) ;
#1331 = CARTESIAN_POINT ( 'NONE',  ( 31.49298359385885959, -60.71197230342421136, 3.050751728647414840 ) ) ;
#1332 = DIRECTION ( 'NONE',  ( -1.000000000000000000, -8.673617379884035472E-17, 0.000000000000000000 ) ) ;
#1333 = CARTESIAN_POINT ( 'NONE',  ( 32.86037637810374434, -54.05488119003602776, -2.185023599737637490 ) ) ;
#1334 = ORIENTED_EDGE ( 'NONE', *, *, #12288, .T. ) ;
#1335 = EDGE_CURVE ( 'NONE', #6376, #5507, #5755, .T. ) ;
#1336 = ORIENTED_EDGE ( 'NONE', *, *, #11677, .F. ) ;
#1337 = FACE_OUTER_BOUND ( 'NONE', #5812, .T. ) ;
#1338 = ORIENTED_EDGE ( 'NONE', *, *, #1702, .T. ) ;
#1339 = LINE ( 'NONE', #187, #12832 ) ;
#1340 = DIRECTION ( 'NONE',  ( 1.000000000000000000, 0.000000000000000000, 0.000000000000000000 ) ) ;
#1341 = ORIENTED_EDGE ( 'NONE', *, *, #987, .F. ) ;
#1342 = CARTESIAN_POINT ( 'NONE',  ( 60.65595175199513278, -6.557103238384438981, 62.84860122826521689 ) ) ;
#1343 = CARTESIAN_POINT ( 'NONE',  ( -8.537170960192327129, 2.067018546614582508, 57.50000000000012079 ) ) ;
#1344 = CARTESIAN_POINT ( 'NONE',  ( 70.18595114983344274, -3.932849470457435714, 76.10019179193449190 ) ) ;
#1345 = CARTESIAN_POINT ( 'NONE',  ( -12.99999999999998757, -2.249290599286444703, -32.99999999999987921 ) ) ;
#1346 = EDGE_CURVE ( 'NONE', #358, #13613, #648, .T. ) ;
#1347 = DIRECTION ( 'NONE',  ( -0.000000000000000000, -0.000000000000000000, -1.000000000000000000 ) ) ;
#1348 = DIRECTION ( 'NONE',  ( -0.000000000000000000, 0.000000000000000000, -1.000000000000000000 ) ) ;
#1349 = EDGE_CURVE ( 'NONE', #4027, #4392, #4504, .T. ) ;
#1350 = CARTESIAN_POINT ( 'NONE',  ( 80.00000000000001421, -85.24929059928629727, 8.000000000000001776 ) ) ;
#1351 = ORIENTED_EDGE ( 'NONE', *, *, #12911, .T. ) ;
#1352 = DIRECTION ( 'NONE',  ( 0.000000000000000000, 1.000000000000000000, -0.000000000000000000 ) ) ;
#1353 = PRODUCT_DEFINITION_CONTEXT ( 'detailed design', #5158, 'design' ) ;
#1354 = ORIENTED_EDGE ( 'NONE', *, *, #14964, .T. ) ;
#1355 = DIRECTION ( 'NONE',  ( 0.000000000000000000, 1.000000000000000000, -0.000000000000000000 ) ) ;
#1356 = ORIENTED_EDGE ( 'NONE', *, *, #9741, .T. ) ;
#1357 = ORIENTED_EDGE ( 'NONE', *, *, #5945, .T. ) ;
#1358 = CARTESIAN_POINT ( 'NONE',  ( 65.71319926014257362, -10.73129157630436659, 77.19766410831375936 ) ) ;
#1359 = DIRECTION ( 'NONE',  ( 1.000000000000000000, 0.000000000000000000, 0.000000000000000000 ) ) ;
#1360 = CYLINDRICAL_SURFACE ( 'NONE', #11358, 10.00000000000000178 ) ;
#1361 = EDGE_CURVE ( 'NONE', #6460, #12669, #7742, .T. ) ;
#1362 = FACE_OUTER_BOUND ( 'NONE', #1607, .T. ) ;
#1363 = DIRECTION ( 'NONE',  ( 0.000000000000000000, 0.000000000000000000, 1.000000000000000000 ) ) ;
#1364 = EDGE_CURVE ( 'NONE', #11647, #12323, #3195, .T. ) ;
#1365 = EDGE_CURVE ( 'NONE', #8543, #4896, #11578, .T. ) ;
#1366 = LINE ( 'NONE', #2596, #12722 ) ;
#1367 = ORIENTED_EDGE ( 'NONE', *, *, #15114, .T. ) ;
#1368 = ORIENTED_EDGE ( 'NONE', *, *, #8899, .T. ) ;
#1369 = CARTESIAN_POINT ( 'NONE',  ( 59.06137132172460014, 0.3483485318593032565, -33.00000000000012790 ) ) ;
#1370 = EDGE_LOOP ( 'NONE', ( #3463, #12064, #11267, #9958 ) ) ;
#1371 = CARTESIAN_POINT ( 'NONE',  ( 12.91143137450191247, -63.78335865426897300, 4.036657210498128201 ) ) ;
#1372 = ORIENTED_EDGE ( 'NONE', *, *, #3914, .F. ) ;
#1373 = CARTESIAN_POINT ( 'NONE',  ( 14.12076545371521519, -53.27034158699100175, 4.884662653952321243 ) ) ;
#1374 = AXIS2_PLACEMENT_3D ( 'NONE', #6468, #8766, #7549 ) ;
#1375 = VERTEX_POINT ( 'NONE', #4186 ) ;
#1376 = LINE ( 'NONE', #7228, #11447 ) ;
#1377 = DIRECTION ( 'NONE',  ( 0.000000000000000000, 0.000000000000000000, 1.000000000000000000 ) ) ;
#1378 = ORIENTED_EDGE ( 'NONE', *, *, #14002, .T. ) ;
#1379 = DIRECTION ( 'NONE',  ( 0.000000000000000000, -1.000000000000000000, 0.000000000000000000 ) ) ;
#1380 = CARTESIAN_POINT ( 'NONE',  ( 59.31076468612580754, 2.638779099491020297, 48.51982618741349285 ) ) ;
#1381 = EDGE_LOOP ( 'NONE', ( #15083, #10267, #135, #6493 ) ) ;
#1382 = EDGE_CURVE ( 'NONE', #13652, #4131, #6504, .T. ) ;
#1383 = VECTOR ( 'NONE', #1822, 1000.000000000000000 ) ;
#1384 = LINE ( 'NONE', #457, #2184 ) ;
#1385 = LINE ( 'NONE', #5078, #7650 ) ;
#1386 = EDGE_CURVE ( 'NONE', #5719, #5462, #7705, .T. ) ;
#1387 = ADVANCED_FACE ( 'NONE', ( #12279 ), #6653, .F. ) ;
#1388 = DIRECTION ( 'NONE',  ( -0.4543483311474630915, 0.8908241094534405935, -0.000000000000000000 ) ) ;
#1389 = ORIENTED_EDGE ( 'NONE', *, *, #12424, .F. ) ;
#1390 = CARTESIAN_POINT ( 'NONE',  ( -24.54301448188264700, 2.673459138797629198, 47.50000001881890910 ) ) ;
#1391 = ORIENTED_EDGE ( 'NONE', *, *, #13173, .T. ) ;
#1392 = FACE_OUTER_BOUND ( 'NONE', #11151, .T. ) ;
#1393 = CIRCLE ( 'NONE', #3357, 9.000000000000001776 ) ;
#1394 = ORIENTED_EDGE ( 'NONE', *, *, #6976, .F. ) ;
#1395 = AXIS2_PLACEMENT_3D ( 'NONE', #2267, #15123, #11570 ) ;
#1396 = PRODUCT_CONTEXT ( 'NONE', #857, 'mechanical' ) ;
#1397 = DIRECTION ( 'NONE',  ( 1.000000000000000000, 1.156482317317870492E-16, 0.000000000000000000 ) ) ;
#1398 = DIRECTION ( 'NONE',  ( 0.000000000000000000, 1.000000000000000000, -0.000000000000000000 ) ) ;
#1399 = CARTESIAN_POINT ( 'NONE',  ( -9.209612907684750382, 2.258800220783480750, -47.62582736825572738 ) ) ;
#1400 = CARTESIAN_POINT ( 'NONE',  ( 9.495483015351213751, -60.90019506145881678, 2.720530867599800562 ) ) ;
#1401 = VECTOR ( 'NONE', #6292, 1000.000000000000000 ) ;
#1402 = DIRECTION ( 'NONE',  ( 1.000000000000000000, 0.000000000000000000, 0.000000000000000000 ) ) ;
#1403 = DIRECTION ( 'NONE',  ( 0.000000000000000000, 0.000000000000000000, -1.000000000000000000 ) ) ;
#1404 = DIRECTION ( 'NONE',  ( 0.8746197071345563900, -0.4848096202550675193, 0.000000000000000000 ) ) ;
#1405 = CARTESIAN_POINT ( 'NONE',  ( 33.46718823248610875, -55.33425260370049870, -2.693485533442558033 ) ) ;
#1406 = CIRCLE ( 'NONE', #12459, 4.999999999999997335 ) ;
#1407 = ADVANCED_FACE ( 'NONE', ( #7894 ), #8810, .F. ) ;
#1408 = CARTESIAN_POINT ( 'NONE',  ( 69.46454297106444642, -2.294433322023680333, 82.40005259842790508 ) ) ;
#1409 = AXIS2_PLACEMENT_3D ( 'NONE', #11979, #4986, #10916 ) ;
#1410 = EDGE_LOOP ( 'NONE', ( #8484, #1826, #6584, #10863 ) ) ;
#1411 = DIRECTION ( 'NONE',  ( 0.000000000000000000, 0.000000000000000000, -1.000000000000000000 ) ) ;
#1412 = CARTESIAN_POINT ( 'NONE',  ( 32.31153295206774345, -59.69665779701220032, -2.790274538705360019 ) ) ;
#1413 = CARTESIAN_POINT ( 'NONE',  ( 80.00000000000001421, -76.24929059928631148, -6.000000000000000000 ) ) ;
#1414 = CARTESIAN_POINT ( 'NONE',  ( 35.49198652140812982, 23.25070940071368852, -33.00000000000012790 ) ) ;
#1415 = AXIS2_PLACEMENT_3D ( 'NONE', #1771, #6471, #12394 ) ;
#1416 = CIRCLE ( 'NONE', #14450, 12.46463184759105047 ) ;
#1417 = FACE_OUTER_BOUND ( 'NONE', #2786, .T. ) ;
#1418 = CARTESIAN_POINT ( 'NONE',  ( -16.99999999999998579, -6.754727345143736628, 36.00000000000012079 ) ) ;
#1419 = EDGE_CURVE ( 'NONE', #3763, #13687, #1067, .T. ) ;
#1420 = CARTESIAN_POINT ( 'NONE',  ( 65.61961478802662384, -10.81639363244362428, 72.15687421485361597 ) ) ;
#1421 = CARTESIAN_POINT ( 'NONE',  ( -24.90214939295363550, -6.558472524147630267, 47.52616914649232172 ) ) ;
#1422 = AXIS2_PLACEMENT_3D ( 'NONE', #9838, #14588, #4037 ) ;
#1423 = AXIS2_PLACEMENT_3D ( 'NONE', #6574, #5131, #1812 ) ;
#1424 = CARTESIAN_POINT ( 'NONE',  ( 32.75756170203653284, -53.92993659400953277, 2.218374547572117716 ) ) ;
#1425 = AXIS2_PLACEMENT_3D ( 'NONE', #6810, #4505, #5756 ) ;
#1426 = ORIENTED_EDGE ( 'NONE', *, *, #10139, .F. ) ;
#1427 = DIRECTION ( 'NONE',  ( 0.000000000000000000, 0.000000000000000000, -1.000000000000000000 ) ) ;
#1428 =( REPRESENTATION_RELATIONSHIP ('NONE','NONE', #15125, #10411 ) REPRESENTATION_RELATIONSHIP_WITH_TRANSFORMATION ( #1554 )SHAPE_REPRESENTATION_RELATIONSHIP( ) );
#1429 = EDGE_LOOP ( 'NONE', ( #13416, #7963, #11470, #145 ) ) ;
#1430 = EDGE_CURVE ( 'NONE', #4665, #307, #15084, .T. ) ;
#1431 = LINE ( 'NONE', #1654, #13791 ) ;
#1432 = ADVANCED_FACE ( 'NONE', ( #12427 ), #1879, .F. ) ;
#1433 = EDGE_LOOP ( 'NONE', ( #6266, #13083, #3751, #10819 ) ) ;
#1435 = ORIENTED_EDGE ( 'NONE', *, *, #5988, .T. ) ;
#1434 = CARTESIAN_POINT ( 'NONE',  ( 32.90197589884652274, -57.33450387999030795, -2.749014434309867916 ) ) ;
#1436 = FACE_OUTER_BOUND ( 'NONE', #5190, .T. ) ;
#1437 = CIRCLE ( 'NONE', #6552, 0.5000000000000004441 ) ;
#1438 = CARTESIAN_POINT ( 'NONE',  ( 58.00000000000000711, 0.000000000000000000, 33.00000000000012790 ) ) ;
#1439 = CIRCLE ( 'NONE', #5620, 1.000000000000001998 ) ;
#1440 = ORIENTED_EDGE ( 'NONE', *, *, #2063, .F. ) ;
#1441 = VERTEX_POINT ( 'NONE', #10128 ) ;
#1442 = CARTESIAN_POINT ( 'NONE',  ( 8.406258358832010558, -54.90785108970787576, 2.018552575025332363 ) ) ;
#1443 = CARTESIAN_POINT ( 'NONE',  ( -80.00000000000001421, -76.24929059928631148, -6.000000000000000000 ) ) ;
#1444 = LINE ( 'NONE', #4764, #6559 ) ;
#1445 = ORIENTED_EDGE ( 'NONE', *, *, #12870, .T. ) ;
#1446 = VERTEX_POINT ( 'NONE', #7822 ) ;
#1447 = CARTESIAN_POINT ( 'NONE',  ( 65.71319926014255941, -10.73129157630437547, 77.19766410831374515 ) ) ;
#1448 = ORIENTED_EDGE ( 'NONE', *, *, #8487, .F. ) ;
#1449 = DIRECTION ( 'NONE',  ( -0.000000000000000000, 0.000000000000000000, -1.000000000000000000 ) ) ;
#1450 = ORIENTED_EDGE ( 'NONE', *, *, #5868, .T. ) ;
#1451 = CARTESIAN_POINT ( 'NONE',  ( 27.60446587309679956, -53.27035316348869998, 4.884032402486375268 ) ) ;
#1452 = AXIS2_PLACEMENT_3D ( 'NONE', #11065, #9559, #2549 ) ;
#1453 = ORIENTED_EDGE ( 'NONE', *, *, #4286, .F. ) ;
#1454 = CARTESIAN_POINT ( 'NONE',  ( -16.99999999999998579, -2.249290599286303927, -47.50000000000012079 ) ) ;
#1455 = CARTESIAN_POINT ( 'NONE',  ( -11.05444845021228595, -9.014367880605227867, 48.04486892757390848 ) ) ;
#1456 = ORIENTED_EDGE ( 'NONE', *, *, #10701, .T. ) ;
#1457 = EDGE_CURVE ( 'NONE', #3968, #9234, #11416, .T. ) ;
#1458 = CARTESIAN_POINT ( 'NONE',  ( -3.285520523750506516, 5.681530634152946568, 48.00000000000012079 ) ) ;
#1459 = DIRECTION ( 'NONE',  ( 0.8746197071345569451, -0.4848096202550666312, 0.000000000000000000 ) ) ;
#1460 = VERTEX_POINT ( 'NONE', #804 ) ;
#1461 = ADVANCED_FACE ( 'NONE', ( #5517 ), #4343, .T. ) ;
#1462 =( BOUNDED_SURFACE ( )  B_SPLINE_SURFACE ( 3, 2, ( 
 ( #5640, #10330, #9182 ),
 ( #13867, #8020, #12719 ),
 ( #5726, #9253, #13947 ),
 ( #8099, #12800, #14104 ),
 ( #2402, #10482, #11935 ),
 ( #11708, #253, #13104 ),
 ( #10566, #3556, #4711 ),
 ( #9573, #2479, #10713 ) ),
 .UNSPECIFIED., .F., .F., .F. ) 
 B_SPLINE_SURFACE_WITH_KNOTS ( ( 4, 2, 2, 4 ),
 ( 3, 3 ),
 ( -6.505213034913026604E-19, 0.001129222206655588513, 0.002258444413311177894, 0.004516888826622356655 ),
 ( 0.000000000000000000, 1.000000000000000000 ),
 .UNSPECIFIED. ) 
 GEOMETRIC_REPRESENTATION_ITEM ( )  RATIONAL_B_SPLINE_SURFACE ( (
 ( 1.000000000000000000, 0.7071067811864926167, 1.000000000000000000),
 ( 1.000000000000000000, 0.7608707698419998611, 1.000000000000000000),
 ( 1.000000000000000000, 0.8047257278452493168, 1.000000000000000000),
 ( 1.000000000000000000, 0.8783509392183369568, 1.000000000000000000),
 ( 1.000000000000000000, 0.9081758943107525184, 1.000000000000000000),
 ( 1.000000000000000000, 0.9781389570701306546, 1.000000000000000000),
 ( 1.000000000000000000, 0.9996704379322433054, 1.000000000000000000),
 ( 1.000000000000000000, 1.000000000000000000, 1.000000000000000000) ) ) 
 REPRESENTATION_ITEM ( '' )  SURFACE ( )  );
#1463 = AXIS2_PLACEMENT_3D ( 'NONE', #12026, #14631, #552 ) ;
#1464 = FACE_OUTER_BOUND ( 'NONE', #14437, .T. ) ;
#1465 = DIRECTION ( 'NONE',  ( 0.000000000000000000, -1.000000000000000000, 0.000000000000000000 ) ) ;
#1466 = DIRECTION ( 'NONE',  ( -1.000000000000000000, -0.000000000000000000, -0.000000000000000000 ) ) ;
#1467 = ORIENTED_EDGE ( 'NONE', *, *, #4385, .F. ) ;
#1468 = CARTESIAN_POINT ( 'NONE',  ( -0.9277479332649583021, -2.641590149077306826, -48.00000000000012079 ) ) ;
#1469 = ORIENTED_EDGE ( 'NONE', *, *, #9614, .T. ) ;
#1470 = DIRECTION ( 'NONE',  ( -0.8208219420614785156, 0.4549890321264269399, 0.3453061251629920836 ) ) ;
#1471 = VECTOR ( 'NONE', #995, 1000.000000000000000 ) ;
#1472 = CARTESIAN_POINT ( 'NONE',  ( 54.85055839958032209, 21.75070940071329417, -33.00000000000012790 ) ) ;
#1473 = AXIS2_PLACEMENT_3D ( 'NONE', #2874, #6349, #7729 ) ;
#1474 = VERTEX_POINT ( 'NONE', #878 ) ;
#1475 = EDGE_CURVE ( 'NONE', #2336, #8264, #13597, .T. ) ;
#1476 = DIRECTION ( 'NONE',  ( 1.000000000000000000, 0.000000000000000000, 0.000000000000000000 ) ) ;
#1477 = CARTESIAN_POINT ( 'NONE',  ( 8.199792978590130232, -57.47994873761393109, 2.501453769636607039 ) ) ;
#1478 = CARTESIAN_POINT ( 'NONE',  ( 63.03271294676726910, -4.597264848142483373, 60.61639468829817190 ) ) ;
#1479 = EDGE_CURVE ( 'NONE', #5596, #6896, #5906, .T. ) ;
#1480 = DIRECTION ( 'NONE',  ( -0.000000000000000000, 1.000000000000000000, 1.445602896647339163E-16 ) ) ;
#1481 = CARTESIAN_POINT ( 'NONE',  ( 18.13205847682796090, -57.03285117767145351, 6.445925775545124914 ) ) ;
#1482 = CARTESIAN_POINT ( 'NONE',  ( 0.000000000000000000, 25.52935533987996664, 0.000000000000000000 ) ) ;
#1483 = CYLINDRICAL_SURFACE ( 'NONE', #13489, 5.496540510819668768 ) ;
#1484 = CARTESIAN_POINT ( 'NONE',  ( -25.01741698508091005, -6.338425579613558014, 47.50000000000012079 ) ) ;
#1485 = CIRCLE ( 'NONE', #9354, 0.5000000000000001110 ) ;
#1486 = CARTESIAN_POINT ( 'NONE',  ( 31.69252035015315627, -52.93050895625588481, -3.457921359511734849 ) ) ;
#1487 = B_SPLINE_CURVE_WITH_KNOTS ( 'NONE', 3,
 ( #955, #15051, #12505, #10283, #5585, #3191, #11341, #12663, #7819, #14971 ),
 .UNSPECIFIED., .F., .F.,
 ( 4, 2, 2, 2, 4 ),
 ( 0.000000000000000000, 0.0004999547661763323846, 0.0009999095323526647691, 0.001499864298528997154, 0.001999819064705329538 ),
 .UNSPECIFIED. ) ;
#1488 = CARTESIAN_POINT ( 'NONE',  ( -9.263396839842437558, 2.349907881949450772, 47.70033363922482295 ) ) ;
#1489 = ORIENTED_EDGE ( 'NONE', *, *, #10313, .T. ) ;
#1490 = DIRECTION ( 'NONE',  ( -0.000000000000000000, 1.000000000000000000, -0.000000000000000000 ) ) ;
#1491 = CARTESIAN_POINT ( 'NONE',  ( 65.00000000000001421, -85.24929059928629727, -22.52499999999999503 ) ) ;
#1492 = EDGE_CURVE ( 'NONE', #4595, #14705, #4581, .T. ) ;
#1493 =( LENGTH_UNIT ( ) NAMED_UNIT ( * ) SI_UNIT ( .MILLI., .METRE. ) );
#1494 = DIRECTION ( 'NONE',  ( 0.000000000000000000, 0.000000000000000000, 1.000000000000000000 ) ) ;
#1495 = CIRCLE ( 'NONE', #10091, 2.000000000000000000 ) ;
#1496 = CARTESIAN_POINT ( 'NONE',  ( 69.44353280118474459, -3.136524796243262525, 75.86075339999212019 ) ) ;
#1497 = LINE ( 'NONE', #348, #6923 ) ;
#1498 = CARTESIAN_POINT ( 'NONE',  ( 64.55850009422569258, -11.65316488165094100, 71.85201186900997072 ) ) ;
#1499 = DIRECTION ( 'NONE',  ( 0.000000000000000000, 0.000000000000000000, 1.000000000000000000 ) ) ;
#1500 = CARTESIAN_POINT ( 'NONE',  ( 55.86211336638498182, 2.337731330496643167, 48.51982618741349285 ) ) ;
#1501 = AXIS2_PLACEMENT_3D ( 'NONE', #5150, #14538, #4054 ) ;
#1502 = CARTESIAN_POINT ( 'NONE',  ( 69.45547845231760675, -2.986442851882156191, 72.75847651673318239 ) ) ;
#1503 = ORIENTED_EDGE ( 'NONE', *, *, #6773, .T. ) ;
#1504 = DIRECTION ( 'NONE',  ( -1.000000000000000000, 0.000000000000000000, 0.000000000000000000 ) ) ;
#1505 = UNCERTAINTY_MEASURE_WITH_UNIT (LENGTH_MEASURE( 1.000000000000000082E-05 ), #623, 'distance_accuracy_value', 'NONE');
#1506 = VERTEX_POINT ( 'NONE', #8049 ) ;
#1507 = CARTESIAN_POINT ( 'NONE',  ( -25.34493114703935035, -6.799303420495464323, 48.05421924268924272 ) ) ;
#1508 = VERTEX_POINT ( 'NONE', #5589 ) ;
#1509 = ORIENTED_EDGE ( 'NONE', *, *, #11188, .T. ) ;
#1510 = AXIS2_PLACEMENT_3D ( 'NONE', #4667, #12835, #13133 ) ;
#1511 = CARTESIAN_POINT ( 'NONE',  ( 35.49198652140812982, 21.75070940071315562, -33.00000000000012790 ) ) ;
#1512 = DIRECTION ( 'NONE',  ( 0.000000000000000000, -1.000000000000000000, 0.000000000000000000 ) ) ;
#1513 = AXIS2_PLACEMENT_3D ( 'NONE', #564, #3097, #1718 ) ;
#1514 = CIRCLE ( 'NONE', #8871, 2.000000000000000000 ) ;
#1515 = CARTESIAN_POINT ( 'NONE',  ( -32.80254285330626374, -2.278009980413909563, 48.00000000000012079 ) ) ;
#1516 = ORIENTED_EDGE ( 'NONE', *, *, #409, .F. ) ;
#1517 = CARTESIAN_POINT ( 'NONE',  ( 8.129887667336562984, -57.17459804181999772, 2.501046471591553466 ) ) ;
#1518 = EDGE_CURVE ( 'NONE', #5832, #10536, #14827, .T. ) ;
#1519 = EDGE_CURVE ( 'NONE', #14965, #977, #1110, .T. ) ;
#1520 = DIRECTION ( 'NONE',  ( -0.000000000000000000, -0.000000000000000000, -1.000000000000000000 ) ) ;
#1521 = AXIS2_PLACEMENT_3D ( 'NONE', #2798, #342, #6267 ) ;
#1522 = CIRCLE ( 'NONE', #14296, 10.00000000000000178 ) ;
#1523 = CYLINDRICAL_SURFACE ( 'NONE', #3638, 0.7892041907098262810 ) ;
#1524 = EDGE_LOOP ( 'NONE', ( #11746, #12539, #5464, #7230 ) ) ;
#1525 = ORIENTED_EDGE ( 'NONE', *, *, #2199, .T. ) ;
#1526 = CARTESIAN_POINT ( 'NONE',  ( 64.11356537587556659, -11.94785244090457965, 75.32972112861136793 ) ) ;
#1527 = VERTEX_POINT ( 'NONE', #957 ) ;
#1528 = EDGE_LOOP ( 'NONE', ( #1020, #1525, #5297, #14230 ) ) ;
#1529 = EDGE_CURVE ( 'NONE', #4620, #12466, #3431, .T. ) ;
#1530 = LINE ( 'NONE', #1675, #8433 ) ;
#1531 = EDGE_LOOP ( 'NONE', ( #3137, #10096, #134, #7878 ) ) ;
#1532 = CARTESIAN_POINT ( 'NONE',  ( 30.59344312246462394, -62.42480215138191113, 2.585081138710340731 ) ) ;
#1533 = ORIENTED_EDGE ( 'NONE', *, *, #8483, .T. ) ;
#1534 = AXIS2_PLACEMENT_3D ( 'NONE', #5720, #3320, #6855 ) ;
#1535 = DIRECTION ( 'NONE',  ( 0.8746197071345569451, -0.4848096202550666312, 0.000000000000000000 ) ) ;
#1536 = LINE ( 'NONE', #2764, #13361 ) ;
#1537 = ORIENTED_EDGE ( 'NONE', *, *, #6853, .F. ) ;
#1538 = VECTOR ( 'NONE', #4607, 1000.000000000000000 ) ;
#1539 = VECTOR ( 'NONE', #8765, 1000.000000000000000 ) ;
#1540 = CARTESIAN_POINT ( 'NONE',  ( 28.60124718008471234, -65.57050171853261133, -4.044987206835048532 ) ) ;
#1541 = ORIENTED_EDGE ( 'NONE', *, *, #13654, .F. ) ;
#1542 = CARTESIAN_POINT ( 'NONE',  ( 26.26264421955999140, -69.39711819508849544, -5.076148092048929250 ) ) ;
#1543 = CARTESIAN_POINT ( 'NONE',  ( -25.49999999999998934, -2.249290599286304815, -38.50000000000012790 ) ) ;
#1544 = DIRECTION ( 'NONE',  ( -0.000000000000000000, 0.000000000000000000, 1.000000000000000000 ) ) ;
#1545 = EDGE_LOOP ( 'NONE', ( #14504, #787, #1294, #11197 ) ) ;
#1546 = AXIS2_PLACEMENT_3D ( 'NONE', #1693, #10005, #10080 ) ;
#1547 = DIRECTION ( 'NONE',  ( -1.000000000000000000, 0.000000000000000000, 0.000000000000000000 ) ) ;
#1548 = ADVANCED_FACE ( 'NONE', ( #8125 ), #12828, .F. ) ;
#1549 = VERTEX_POINT ( 'NONE', #10515 ) ;
#1550 = ORIENTED_EDGE ( 'NONE', *, *, #14612, .F. ) ;
#1551 = VECTOR ( 'NONE', #10800, 1000.000000000000000 ) ;
#1552 = CARTESIAN_POINT ( 'NONE',  ( 80.00000000000001421, -76.24929059928631148, -4.000000000000000000 ) ) ;
#1553 = ORIENTED_EDGE ( 'NONE', *, *, #485, .T. ) ;
#1554 = ITEM_DEFINED_TRANSFORMATION ( 'NONE', 'NONE', #1156,  #6315 ) ;
#1555 = CARTESIAN_POINT ( 'NONE',  ( 0.000000000000000000, 21.75070940071369918, -33.00000000000012790 ) ) ;
#1556 = LINE ( 'NONE', #5543, #8188 ) ;
#1557 = SHAPE_REPRESENTATION ( 'Simple Mounting Plate', ( #6315 ), #10740 ) ;
#1558 = DIRECTION ( 'NONE',  ( 0.000000000000000000, -1.000000000000000000, 0.000000000000000000 ) ) ;
#1559 = ORIENTED_EDGE ( 'NONE', *, *, #10247, .T. ) ;
#1560 = CARTESIAN_POINT ( 'NONE',  ( 12.72502611717542109, -51.89470720432451145, 4.215327498671517681 ) ) ;
#1561 = CIRCLE ( 'NONE', #6462, 7.000000000000000000 ) ;
#1562 = CARTESIAN_POINT ( 'NONE',  ( 67.21328690825531282, 22.43695620243006772, -33.00000000000012790 ) ) ;
#1563 = AXIS2_PLACEMENT_3D ( 'NONE', #4624, #8170, #11384 ) ;
#1564 = DIRECTION ( 'NONE',  ( -0.000000000000000000, -0.000000000000000000, 1.000000000000000000 ) ) ;
#1565 = CARTESIAN_POINT ( 'NONE',  ( 32.09878978612020006, -53.24145049768157634, -2.425475548245525470 ) ) ;
#1566 = EDGE_CURVE ( 'NONE', #2463, #8222, #8929, .T. ) ;
#1567 = EDGE_CURVE ( 'NONE', #3404, #4646, #2275, .T. ) ;
#1568 = CARTESIAN_POINT ( 'NONE',  ( -9.191242442328487527, 2.249476921181321476, 48.36238429206942868 ) ) ;
#1569 = ORIENTED_EDGE ( 'NONE', *, *, #12912, .F. ) ;
#1570 = CARTESIAN_POINT ( 'NONE',  ( 30.65234355186507997, 21.75070940071312364, -33.00000000000012790 ) ) ;
#1571 =( NAMED_UNIT ( * ) PLANE_ANGLE_UNIT ( ) SI_UNIT ( $, .RADIAN. ) );
#1572 = CARTESIAN_POINT ( 'NONE',  ( 17.61519226005271577, -69.39711819508849544, 6.201611931792121446 ) ) ;
#1573 = AXIS2_PLACEMENT_3D ( 'NONE', #13753, #7834, #7985 ) ;
#1574 = CARTESIAN_POINT ( 'NONE',  ( 69.44830357739648719, -3.079170558718888007, 75.78944312221568680 ) ) ;
#1575 = CARTESIAN_POINT ( 'NONE',  ( 58.00000000000000711, -12.24929059928630970, 33.00000000000012790 ) ) ;
#1576 = CARTESIAN_POINT ( 'NONE',  ( -6.999999999999978684, -69.24929059928631148, -32.99999999999999289 ) ) ;
#1577 = FACE_OUTER_BOUND ( 'NONE', #10763, .T. ) ;
#1578 = EDGE_CURVE ( 'NONE', #10002, #10908, #7906, .T. ) ;
#1579 = EDGE_CURVE ( 'NONE', #7961, #60, #5669, .T. ) ;
#1580 = VERTEX_POINT ( 'NONE', #13813 ) ;
#1581 = CARTESIAN_POINT ( 'NONE',  ( 112.9262740340969060, 0.000000000000000000, -33.00000000000012790 ) ) ;
#1582 = VERTEX_POINT ( 'NONE', #3277 ) ;
#1583 = CARTESIAN_POINT ( 'NONE',  ( 18.00000000000001066, 0.000000000000000000, -33.00000000000012790 ) ) ;
#1584 = DIRECTION ( 'NONE',  ( -1.000000000000000000, -0.000000000000000000, -0.000000000000000000 ) ) ;
#1585 = VERTEX_POINT ( 'NONE', #7975 ) ;
#1587 = VERTEX_POINT ( 'NONE', #4661 ) ;
#1586 = CARTESIAN_POINT ( 'NONE',  ( 58.92629142760363692, 23.25070940071368852, 84.20452624982236500 ) ) ;
#1588 = DIRECTION ( 'NONE',  ( 0.000000000000000000, 0.000000000000000000, -1.000000000000000000 ) ) ;
#1589 = PLANE ( 'NONE',  #10650 ) ;
#1590 = ORIENTED_EDGE ( 'NONE', *, *, #13873, .F. ) ;
#1591 = CARTESIAN_POINT ( 'NONE',  ( 9.216223969337589139, -54.89772082965570377, 3.066133849897938468 ) ) ;
#1592 = DIRECTION ( 'NONE',  ( 1.734723475976807094E-15, 0.000000000000000000, -1.000000000000000000 ) ) ;
#1593 = CARTESIAN_POINT ( 'NONE',  ( 112.9262740340969060, 0.000000000000000000, 33.00000000000012790 ) ) ;
#1594 = ORIENTED_EDGE ( 'NONE', *, *, #4562, .T. ) ;
#1595 = ORIENTED_EDGE ( 'NONE', *, *, #14496, .F. ) ;
#1596 = CARTESIAN_POINT ( 'NONE',  ( 8.599030766203958009, -59.21224831720011395, 2.500000000000000000 ) ) ;
#1597 = ADVANCED_FACE ( 'NONE', ( #2113 ), #10588, .F. ) ;
#1598 = ORIENTED_EDGE ( 'NONE', *, *, #5035, .T. ) ;
#1599 = FACE_OUTER_BOUND ( 'NONE', #1545, .T. ) ;
#1600 = VERTEX_POINT ( 'NONE', #15053 ) ;
#1601 = DIRECTION ( 'NONE',  ( 0.9816271834495682302, 0.1908089953667485572, 0.000000000000000000 ) ) ;
#1602 = ORIENTED_EDGE ( 'NONE', *, *, #13204, .F. ) ;
#1603 = EDGE_CURVE ( 'NONE', #13714, #11917, #14688, .T. ) ;
#1604 = EDGE_CURVE ( 'NONE', #12366, #3697, #9209, .T. ) ;
#1605 = CARTESIAN_POINT ( 'NONE',  ( -8.499999999999987566, -2.249290599286303927, 38.00000000000012079 ) ) ;
#1606 = CARTESIAN_POINT ( 'NONE',  ( -32.80254285330622821, -2.278009980413885582, -58.00000000000012079 ) ) ;
#1607 = EDGE_LOOP ( 'NONE', ( #662, #7615, #7842, #2669, #7464 ) ) ;
#1608 = CARTESIAN_POINT ( 'NONE',  ( 28.20373290646802289, -66.75404937492989177, -3.551013195539084677 ) ) ;
#1609 = EDGE_LOOP ( 'NONE', ( #11446, #15210 ) ) ;
#1610 = ADVANCED_FACE ( 'NONE', ( #5982, #128 ), #1269, .F. ) ;
#1611 = EDGE_CURVE ( 'NONE', #11349, #2219, #7955, .T. ) ;
#1612 = CARTESIAN_POINT ( 'NONE',  ( 21.74884261173415467, -85.24929059928631148, -6.000000000000000888 ) ) ;
#1613 = DIRECTION ( 'NONE',  ( 1.000000000000000000, -2.602085213965208275E-15, 0.000000000000000000 ) ) ;
#1614 = CARTESIAN_POINT ( 'NONE',  ( 114.6731053250840233, 23.25070940071369563, 139.1143251403882459 ) ) ;
#1615 = ORIENTED_EDGE ( 'NONE', *, *, #2520, .F. ) ;
#1616 = CYLINDRICAL_SURFACE ( 'NONE', #11018, 31.00000000000000000 ) ;
#1617 = ORIENTED_EDGE ( 'NONE', *, *, #311, .T. ) ;
#1618 = ORIENTED_EDGE ( 'NONE', *, *, #5942, .F. ) ;
#1619 = EDGE_CURVE ( 'NONE', #10926, #10853, #8787, .T. ) ;
#1620 = DIRECTION ( 'NONE',  ( 1.000000000000000000, 0.000000000000000000, 0.000000000000000000 ) ) ;
#1621 = ADVANCED_FACE ( 'NONE', ( #4560 ), #6714, .T. ) ;
#1622 = APPLICATION_PROTOCOL_DEFINITION ( 'draft international standard', 'automotive_design', 1998, #2001 ) ;
#1623 = FACE_OUTER_BOUND ( 'NONE', #5230, .T. ) ;
#1624 = CARTESIAN_POINT ( 'NONE',  ( -20.99999999999998579, -2.249290599286445591, -32.99999999999987921 ) ) ;
#1625 = CARTESIAN_POINT ( 'NONE',  ( -11.45041300328984413, -9.336677115435668028, -48.21133583021728697 ) ) ;
#1626 = AXIS2_PLACEMENT_3D ( 'NONE', #9334, #2248, #15108 ) ;
#1627 = CARTESIAN_POINT ( 'NONE',  ( 17.45100281819997079, -72.28366650274460881, 6.113054590623445250 ) ) ;
#1628 = CYLINDRICAL_SURFACE ( 'NONE', #13220, 4.505436745857433145 ) ;
#1629 = DIRECTION ( 'NONE',  ( -0.000000000000000000, -0.000000000000000000, 1.000000000000000000 ) ) ;
#1630 = DIRECTION ( 'NONE',  ( 1.000000000000000000, 0.000000000000000000, 0.000000000000000000 ) ) ;
#1631 = CARTESIAN_POINT ( 'NONE',  ( 14.38836832001927846, -69.49659648540917090, -4.497058153269694714 ) ) ;
#1632 = VECTOR ( 'NONE', #13443, 1000.000000000000000 ) ;
#1633 = CIRCLE ( 'NONE', #11945, 0.7892041907098272802 ) ;
#1634 = CARTESIAN_POINT ( 'NONE',  ( -9.198099351547387670, 2.262399358110477543, 48.50000000000012079 ) ) ;
#1635 = ORIENTED_EDGE ( 'NONE', *, *, #471, .T. ) ;
#1636 =( NAMED_UNIT ( * ) SI_UNIT ( $, .STERADIAN. ) SOLID_ANGLE_UNIT ( ) );
#1637 = CARTESIAN_POINT ( 'NONE',  ( -12.41494337171168283, -9.406612424898836977, -57.50000000000012079 ) ) ;
#1638 = SHAPE_REPRESENTATION_RELATIONSHIP ( 'NONE' , 'NONE' ,  #11466, #10707 ) ;
#1639 = CARTESIAN_POINT ( 'NONE',  ( 54.06723705530823310, -0.06932450177430304894, 86.40005259842790508 ) ) ;
#1640 = VECTOR ( 'NONE', #3870, 1000.000000000000000 ) ;
#1641 = CARTESIAN_POINT ( 'NONE',  ( 10.42210623299234840, -53.71252461569496006, 3.555803702006939737 ) ) ;
#1642 = CARTESIAN_POINT ( 'NONE',  ( 64.11356537587560922, -11.94785244090458498, 73.06537742987060824 ) ) ;
#1643 = ADVANCED_FACE ( 'NONE', ( #15110 ), #1014, .F. ) ;
#1644 = AXIS2_PLACEMENT_3D ( 'NONE', #14275, #15068, #3574 ) ;
#1645 = AXIS2_PLACEMENT_3D ( 'NONE', #14043, #15199, #1029 ) ;
#1646 = CARTESIAN_POINT ( 'NONE',  ( 27.48632486622552662, -69.39711819508849544, -4.406545790198922674 ) ) ;
#1647 = CARTESIAN_POINT ( 'NONE',  ( 8.333746554286264541, -58.06117559053629407, -1.821720188324787992 ) ) ;
#1648 = AXIS2_PLACEMENT_3D ( 'NONE', #11908, #9701, #13294 ) ;
#1649 = ORIENTED_EDGE ( 'NONE', *, *, #8333, .T. ) ;
#1650 = DIRECTION ( 'NONE',  ( 0.000000000000000000, 1.000000000000000000, -0.000000000000000000 ) ) ;
#1651 = UNCERTAINTY_MEASURE_WITH_UNIT (LENGTH_MEASURE( 1.000000000000000082E-05 ), #7097, 'distance_accuracy_value', 'NONE');
#1652 = AXIS2_PLACEMENT_3D ( 'NONE', #7089, #5870, #4698 ) ;
#1653 = ORIENTED_EDGE ( 'NONE', *, *, #4198, .F. ) ;
#1654 = CARTESIAN_POINT ( 'NONE',  ( 40.00000000000002132, 23.95881716715919652, 33.00000000000017053 ) ) ;
#1655 = DIRECTION ( 'NONE',  ( -0.000000000000000000, 1.000000000000000000, -0.000000000000000000 ) ) ;
#1656 = EDGE_CURVE ( 'NONE', #12140, #10521, #13236, .T. ) ;
#1657 = AXIS2_PLACEMENT_3D ( 'NONE', #14633, #10959, #8784 ) ;
#1658 = ORIENTED_EDGE ( 'NONE', *, *, #11767, .F. ) ;
#1659 = LINE ( 'NONE', #6354, #12590 ) ;
#1660 = PLANE ( 'NONE',  #10735 ) ;
#1661 = EDGE_CURVE ( 'NONE', #11281, #5785, #1667, .T. ) ;
#1662 = ADVANCED_FACE ( 'NONE', ( #3174 ), #11641, .T. ) ;
#1663 = CARTESIAN_POINT ( 'NONE',  ( -16.99999999999998579, -2.249290599286303927, -50.00000000000012079 ) ) ;
#1664 = VECTOR ( 'NONE', #4909, 1000.000000000000000 ) ;
#1665 = DIRECTION ( 'NONE',  ( 0.000000000000000000, -1.000000000000000000, 0.000000000000000000 ) ) ;
#1666 = AXIS2_PLACEMENT_3D ( 'NONE', #14514, #1665, #8887 ) ;
#1667 = CIRCLE ( 'NONE', #9049, 8.500000000000000000 ) ;
#1668 = VECTOR ( 'NONE', #10391, 1000.000000000000000 ) ;
#1669 = LINE ( 'NONE', #12057, #6239 ) ;
#1670 = DIRECTION ( 'NONE',  ( 0.000000000000000000, 1.000000000000000000, -0.000000000000000000 ) ) ;
#1671 = VERTEX_POINT ( 'NONE', #11398 ) ;
#1672 = ORIENTED_EDGE ( 'NONE', *, *, #10963, .F. ) ;
#1673 = DIRECTION ( 'NONE',  ( 1.000000000000000000, 0.000000000000000000, -0.000000000000000000 ) ) ;
#1674 = ORIENTED_EDGE ( 'NONE', *, *, #3328, .F. ) ;
#1675 = CARTESIAN_POINT ( 'NONE',  ( 120.1999296558884254, -32.15385833656369385, 53.46824312087640863 ) ) ;
#1676 = AXIS2_PLACEMENT_3D ( 'NONE', #10243, #7634, #6541 ) ;
#1677 = ORIENTED_EDGE ( 'NONE', *, *, #13730, .F. ) ;
#1678 = CARTESIAN_POINT ( 'NONE',  ( 17.09549820959326638, -82.24929059928629727, -1.347403282660980528 ) ) ;
#1679 = VERTEX_POINT ( 'NONE', #8025 ) ;
#1680 = CIRCLE ( 'NONE', #6838, 7.924024642120691908 ) ;
#1681 = CARTESIAN_POINT ( 'NONE',  ( 23.36173033120691400, -82.24929059928629727, 6.000000000000001776 ) ) ;
#1682 = CARTESIAN_POINT ( 'NONE',  ( 105.5545870572953930, 15.25070940071369563, -13.14990448602692474 ) ) ;
#1683 = ORIENTED_EDGE ( 'NONE', *, *, #7122, .F. ) ;
#1684 = DIRECTION ( 'NONE',  ( -1.000000000000000000, -0.000000000000000000, -0.000000000000000000 ) ) ;
#1685 = ORIENTED_EDGE ( 'NONE', *, *, #6230, .F. ) ;
#1686 = CARTESIAN_POINT ( 'NONE',  ( -80.00000000000001421, -74.24929059928631148, -8.000000000000001776 ) ) ;
#1687 = CARTESIAN_POINT ( 'NONE',  ( -16.99999999999998579, -2.249290599286303927, 47.50000000000012079 ) ) ;
#1688 = DIRECTION ( 'NONE',  ( 0.000000000000000000, 1.000000000000000000, 1.734723475976807094E-15 ) ) ;
#1689 = EDGE_LOOP ( 'NONE', ( #1895, #13919 ) ) ;
#1690 = DIRECTION ( 'NONE',  ( 0.000000000000000000, -0.000000000000000000, -1.000000000000000000 ) ) ;
#1691 = VERTEX_POINT ( 'NONE', #3410 ) ;
#1692 = ORIENTED_EDGE ( 'NONE', *, *, #11765, .T. ) ;
#1693 = CARTESIAN_POINT ( 'NONE',  ( 58.00000000000000711, -2.249290599286309256, 60.61639468829817190 ) ) ;
#1694 = EDGE_CURVE ( 'NONE', #1089, #7432, #9259, .T. ) ;
#1695 = CARTESIAN_POINT ( 'NONE',  ( 37.90194648202322014, 13.46465865409118834, 89.15517579724127017 ) ) ;
#1696 = DIRECTION ( 'NONE',  ( 0.000000000000000000, 1.000000000000000000, 0.000000000000000000 ) ) ;
#1697 = DIRECTION ( 'NONE',  ( 0.000000000000000000, 1.000000000000000000, -0.000000000000000000 ) ) ;
#1698 = FACE_OUTER_BOUND ( 'NONE', #8312, .T. ) ;
#1699 = CARTESIAN_POINT ( 'NONE',  ( 58.00000000000000711, -2.249290599286311032, 36.00000000000012079 ) ) ;
#1700 = ADVANCED_BREP_SHAPE_REPRESENTATION ( '', ( #9466, #6315 ), #11962 ) ;
#1701 = CARTESIAN_POINT ( 'NONE',  ( 49.07597535787931520, -2.249290599286308368, 39.50000000000012790 ) ) ;
#1702 = EDGE_CURVE ( 'NONE', #3976, #2824, #2890, .T. ) ;
#1703 = CARTESIAN_POINT ( 'NONE',  ( 14.38963276113423895, -69.39711819508849544, 4.502057496415707405 ) ) ;
#1704 = CARTESIAN_POINT ( 'NONE',  ( 18.03113812440136243, 0.000000000000000000, -4.472107801411127959 ) ) ;
#1705 = EDGE_CURVE ( 'NONE', #20, #9290, #6865, .T. ) ;
#1706 = VECTOR ( 'NONE', #9108, 1000.000000000000000 ) ;
#1707 = FACE_OUTER_BOUND ( 'NONE', #14370, .T. ) ;
#1708 = VERTEX_POINT ( 'NONE', #934 ) ;
#1709 = DIRECTION ( 'NONE',  ( -1.000000000000000000, -1.156482317317871725E-16, 0.000000000000000000 ) ) ;
#1710 = FACE_OUTER_BOUND ( 'NONE', #11202, .T. ) ;
#1711 = DIRECTION ( 'NONE',  ( 0.4848096202550661871, 0.8746197071345573892, -0.000000000000000000 ) ) ;
#1712 = ORIENTED_EDGE ( 'NONE', *, *, #14627, .F. ) ;
#1713 = CARTESIAN_POINT ( 'NONE',  ( 33.25707175001029015, -58.63671304798791084, -1.826958385055442058 ) ) ;
#1714 = CARTESIAN_POINT ( 'NONE',  ( -8.982583014919022446, 1.839844381040865118, 47.50000000000012079 ) ) ;
#1715 = CIRCLE ( 'NONE', #13510, 6.000000000000000000 ) ;
#1716 = DIRECTION ( 'NONE',  ( 0.000000000000000000, -1.000000000000000000, -2.312964634635740689E-15 ) ) ;
#1717 = LINE ( 'NONE', #8951, #3460 ) ;
#1718 = DIRECTION ( 'NONE',  ( 0.000000000000000000, 0.000000000000000000, 1.000000000000000000 ) ) ;
#1719 = ORIENTED_EDGE ( 'NONE', *, *, #112, .F. ) ;
#1720 = CARTESIAN_POINT ( 'NONE',  ( 34.73715154119699378, -48.72433491194829713, -2.732636121790667172 ) ) ;
#1721 = EDGE_CURVE ( 'NONE', #13543, #1911, #5496, .T. ) ;
#1722 = ORIENTED_EDGE ( 'NONE', *, *, #13799, .T. ) ;
#1723 = DIRECTION ( 'NONE',  ( 0.8420378618367644341, 0.5394184268574535590, -0.000000000000000000 ) ) ;
#1724 = CARTESIAN_POINT ( 'NONE',  ( 80.00000000000001421, -85.24929059928631148, -6.000000000000001776 ) ) ;
#1725 = CIRCLE ( 'NONE', #14018, 3.000000000000002665 ) ;
#1726 = ORIENTED_EDGE ( 'NONE', *, *, #5264, .F. ) ;
#1728 = ORIENTED_EDGE ( 'NONE', *, *, #247, .T. ) ;
#1727 = CARTESIAN_POINT ( 'NONE',  ( 18.03113812440135888, -82.24929059928629727, -4.472107801411128847 ) ) ;
#1729 = DIRECTION ( 'NONE',  ( -0.5394184268574414576, 0.8420378618367722057, 0.000000000000000000 ) ) ;
#1730 = ORIENTED_EDGE ( 'NONE', *, *, #9732, .T. ) ;
#1731 = CARTESIAN_POINT ( 'NONE',  ( -33.07225206673494711, -1.856991049495498425, -57.50000000000012079 ) ) ;
#1732 = CARTESIAN_POINT ( 'NONE',  ( 11.74003636399016237, -52.28415370497031489, 3.028416065278661584 ) ) ;
#1733 = DIRECTION ( 'NONE',  ( -0.000000000000000000, -0.000000000000000000, -1.000000000000000000 ) ) ;
#1734 = DIRECTION ( 'NONE',  ( 1.000000000000000000, 0.000000000000000000, 0.000000000000000000 ) ) ;
#1735 = ORIENTED_EDGE ( 'NONE', *, *, #8857, .F. ) ;
#1736 = CARTESIAN_POINT ( 'NONE',  ( 9.358332060254376472, -60.82697974174657674, 1.965378744862418925 ) ) ;
#1737 = CIRCLE ( 'NONE', #3474, 4.194885682587998765 ) ;
#1738 = EDGE_CURVE ( 'NONE', #1089, #9843, #11730, .T. ) ;
#1739 = EDGE_CURVE ( 'NONE', #6140, #7395, #10489, .T. ) ;
#1740 = ORIENTED_EDGE ( 'NONE', *, *, #7059, .T. ) ;
#1741 = VERTEX_POINT ( 'NONE', #2017 ) ;
#1742 = CARTESIAN_POINT ( 'NONE',  ( -24.34228330361342785, 2.967490118658024034, 47.54143911729025973 ) ) ;
#1743 = EDGE_LOOP ( 'NONE', ( #3668, #8719, #14872, #8238 ) ) ;
#1744 = DIRECTION ( 'NONE',  ( 0.000000000000000000, 1.000000000000000000, -0.000000000000000000 ) ) ;
#1745 = AXIS2_PLACEMENT_3D ( 'NONE', #3312, #839, #5548 ) ;
#1746 = CARTESIAN_POINT ( 'NONE',  ( 69.30409605188944511, -4.165705203404209023, 71.19766410831373094 ) ) ;
#1747 = CARTESIAN_POINT ( 'NONE',  ( 40.00000000000001421, 23.95881716715930665, -32.99999999999982947 ) ) ;
#1748 = DIRECTION ( 'NONE',  ( -0.5006040828730989878, 0.8656763553492631269, 0.000000000000000000 ) ) ;
#1749 = ORIENTED_EDGE ( 'NONE', *, *, #13506, .F. ) ;
#1750 = CARTESIAN_POINT ( 'NONE',  ( 65.00000000000001421, -87.24929059928631148, -17.50000000000000000 ) ) ;
#1751 = VECTOR ( 'NONE', #2028, 1000.000000000000000 ) ;
#1752 = ORIENTED_EDGE ( 'NONE', *, *, #14178, .F. ) ;
#1753 = CIRCLE ( 'NONE', #2253, 4.194885682587998765 ) ;
#1754 = VECTOR ( 'NONE', #9423, 1000.000000000000000 ) ;
#1755 = CARTESIAN_POINT ( 'NONE',  ( 25.17145219045128712, -52.24929059928630437, 4.731961142181925872 ) ) ;
#1756 = DIRECTION ( 'NONE',  ( 0.000000000000000000, 0.000000000000000000, 1.000000000000000000 ) ) ;
#1757 = DIRECTION ( 'NONE',  ( -0.000000000000000000, -0.000000000000000000, -1.000000000000000000 ) ) ;
#1758 = ORIENTED_EDGE ( 'NONE', *, *, #7122, .T. ) ;
#1759 = EDGE_CURVE ( 'NONE', #12282, #6287, #1910, .T. ) ;
#1760 = FACE_OUTER_BOUND ( 'NONE', #8836, .T. ) ;
#1761 = ORIENTED_EDGE ( 'NONE', *, *, #12757, .T. ) ;
#1762 = VERTEX_POINT ( 'NONE', #4318 ) ;
#1763 = EDGE_LOOP ( 'NONE', ( #8003, #5857, #4349, #10040 ) ) ;
#1764 = VECTOR ( 'NONE', #15120, 1000.000000000000000 ) ;
#1765 = CARTESIAN_POINT ( 'NONE',  ( 54.17164678268019173, 2.103670757168141670, 62.84860122826521689 ) ) ;
#1766 = VECTOR ( 'NONE', #7495, 1000.000000000000000 ) ;
#1767 = DIRECTION ( 'NONE',  ( -0.000000000000000000, 0.000000000000000000, 1.000000000000000000 ) ) ;
#1768 = CARTESIAN_POINT ( 'NONE',  ( 69.97972559857382180, -3.172990593254279457, 0.000000000000000000 ) ) ;
#1769 = DIRECTION ( 'NONE',  ( 0.000000000000000000, 0.000000000000000000, -1.000000000000000000 ) ) ;
#1770 = EDGE_LOOP ( 'NONE', ( #3230, #8616, #5674, #9924 ) ) ;
#1771 = CARTESIAN_POINT ( 'NONE',  ( 58.00000000000000711, -2.249290599286311032, 36.00000000000012079 ) ) ;
#1772 = CARTESIAN_POINT ( 'NONE',  ( 54.00000000000000711, -2.249290599286311032, 139.1143251403882459 ) ) ;
#1773 = AXIS2_PLACEMENT_3D ( 'NONE', #8136, #7618, #11156 ) ;
#1774 = FACE_OUTER_BOUND ( 'NONE', #5288, .T. ) ;
#1775 = TOROIDAL_SURFACE ( 'NONE', #9866, 4.496540510819672321, 1.000000000000000000 ) ;
#1776 = DIRECTION ( 'NONE',  ( 0.000000000000000000, 0.000000000000000000, 1.000000000000000000 ) ) ;
#1777 = CARTESIAN_POINT ( 'NONE',  ( 12.96675353036082257, -65.20845675887582615, -3.989712384465763595 ) ) ;
#1778 = CIRCLE ( 'NONE', #4219, 12.46463184759105047 ) ;
#1779 = ORIENTED_EDGE ( 'NONE', *, *, #6089, .F. ) ;
#1780 = CARTESIAN_POINT ( 'NONE',  ( 33.58103295469781813, -55.84923954203684104, 1.895000442030748022 ) ) ;
#1781 = VECTOR ( 'NONE', #5838, 1000.000000000000000 ) ;
#1782 = CARTESIAN_POINT ( 'NONE',  ( 55.17185982823698964, 2.720345114498381456, 60.61639468829817190 ) ) ;
#1783 = ADVANCED_FACE ( 'NONE', ( #10260 ), #14952, .T. ) ;
#1784 = ORIENTED_EDGE ( 'NONE', *, *, #10860, .F. ) ;
#1785 = CARTESIAN_POINT ( 'NONE',  ( 30.27115683117171585, -61.78784708351293631, -3.496562482608110312 ) ) ;
#1786 = AXIS2_PLACEMENT_3D ( 'NONE', #3044, #13732, #13805 ) ;
#1787 = DIRECTION ( 'NONE',  ( 0.000000000000000000, 0.000000000000000000, 1.000000000000000000 ) ) ;
#1788 = VERTEX_POINT ( 'NONE', #8494 ) ;
#1789 = EDGE_CURVE ( 'NONE', #6376, #7757, #8319, .T. ) ;
#1790 = EDGE_CURVE ( 'NONE', #8955, #2597, #4873, .T. ) ;
#1791 = CARTESIAN_POINT ( 'NONE',  ( 8.782534692662792963, -56.07151166541877529, 2.830535587930131936 ) ) ;
#1792 = EDGE_CURVE ( 'NONE', #7274, #7793, #4055, .T. ) ;
#1793 = AXIS2_PLACEMENT_3D ( 'NONE', #6361, #13067, #12201 ) ;
#1794 = AXIS2_PLACEMENT_3D ( 'NONE', #1663, #5129, #10911 ) ;
#1795 = FACE_OUTER_BOUND ( 'NONE', #4569, .T. ) ;
#1796 = CARTESIAN_POINT ( 'NONE',  ( -8.779641963837230279, 13.70511383897430058, 48.00000000000012079 ) ) ;
#1797 = ADVANCED_FACE ( 'NONE', ( #11713 ), #5355, .T. ) ;
#1798 = CARTESIAN_POINT ( 'NONE',  ( -25.24934951899391322, -6.946659123520668722, -48.24789848114230040 ) ) ;
#1799 = ORIENTED_EDGE ( 'NONE', *, *, #5428, .F. ) ;
#1800 = VECTOR ( 'NONE', #3512, 1000.000000000000000 ) ;
#1801 = CARTESIAN_POINT ( 'NONE',  ( 23.78962786808486740, -62.59345883563879909, -6.358786672826048481 ) ) ;
#1802 = CIRCLE ( 'NONE', #4246, 0.5000000000000000000 ) ;
#1803 = ORIENTED_EDGE ( 'NONE', *, *, #5053, .T. ) ;
#1804 = FACE_BOUND ( 'NONE', #3358, .T. ) ;
#1805 = LINE ( 'NONE', #11184, #8891 ) ;
#1806 = EDGE_LOOP ( 'NONE', ( #9387, #9780, #1784, #11783 ) ) ;
#1807 = LINE ( 'NONE', #637, #3513 ) ;
#1808 = CARTESIAN_POINT ( 'NONE',  ( -8.787473001628837821, 2.499856724289235554, -58.00000000000012079 ) ) ;
#1809 = VERTEX_POINT ( 'NONE', #4945 ) ;
#1810 = EDGE_CURVE ( 'NONE', #304, #9073, #3789, .T. ) ;
#1811 = CARTESIAN_POINT ( 'NONE',  ( 12.23810814295288019, -62.76259148841472069, 3.786770376139185323 ) ) ;
#1812 = DIRECTION ( 'NONE',  ( 0.000000000000000000, -5.204170427930416550E-15, -1.000000000000000000 ) ) ;
#1813 = EDGE_CURVE ( 'NONE', #9234, #13543, #6111, .T. ) ;
#1814 = CARTESIAN_POINT ( 'NONE',  ( 80.00000000000001421, -74.24929059928631148, 32.00000000000000000 ) ) ;
#1815 = FACE_OUTER_BOUND ( 'NONE', #9374, .T. ) ;
#1816 = ORIENTED_EDGE ( 'NONE', *, *, #13193, .F. ) ;
#1817 = CARTESIAN_POINT ( 'NONE',  ( 8.875263511806062766, -60.06858080083353002, 1.862453320361853182 ) ) ;
#1818 = ORIENTED_EDGE ( 'NONE', *, *, #10407, .T. ) ;
#1819 = DIRECTION ( 'NONE',  ( -0.9421718071228326608, -7.134436752378406426E-17, 0.3351302520855077849 ) ) ;
#1820 = ORIENTED_EDGE ( 'NONE', *, *, #3813, .F. ) ;
#1821 = DIRECTION ( 'NONE',  ( 0.000000000000000000, 0.000000000000000000, 1.000000000000000000 ) ) ;
#1822 = DIRECTION ( 'NONE',  ( -0.000000000000000000, -0.000000000000000000, -1.000000000000000000 ) ) ;
#1823 = EDGE_CURVE ( 'NONE', #8849, #1741, #9036, .T. ) ;
#1824 = CARTESIAN_POINT ( 'NONE',  ( 69.46454297106444642, -2.294433322023680333, 75.19766410831374515 ) ) ;
#1825 = DIRECTION ( 'NONE',  ( -1.000000000000000000, -0.000000000000000000, -0.000000000000000000 ) ) ;
#1826 = ORIENTED_EDGE ( 'NONE', *, *, #7252, .T. ) ;
#1827 = LINE ( 'NONE', #519, #6922 ) ;
#1828 = VERTEX_POINT ( 'NONE', #333 ) ;
#1829 = EDGE_CURVE ( 'NONE', #5327, #2379, #178, .T. ) ;
#1830 = ADVANCED_FACE ( 'NONE', ( #8267 ), #6033, .T. ) ;
#1831 = DIRECTION ( 'NONE',  ( 0.000000000000000000, 0.000000000000000000, -1.000000000000000000 ) ) ;
#1832 = LINE ( 'NONE', #823, #803 ) ;
#1833 = DIRECTION ( 'NONE',  ( 0.000000000000000000, 1.000000000000000000, -0.000000000000000000 ) ) ;
#1834 = VERTEX_POINT ( 'NONE', #9654 ) ;
#1835 = DIRECTION ( 'NONE',  ( -0.000000000000000000, -0.000000000000000000, -1.000000000000000000 ) ) ;
#1836 = ORIENTED_EDGE ( 'NONE', *, *, #5241, .F. ) ;
#1837 = ORIENTED_EDGE ( 'NONE', *, *, #7544, .T. ) ;
#1838 = VERTEX_POINT ( 'NONE', #13180 ) ;
#1839 = CARTESIAN_POINT ( 'NONE',  ( 8.599030766203954457, -59.21224831720009973, -1.832439066040443043 ) ) ;
#1840 = CARTESIAN_POINT ( 'NONE',  ( -23.87164973098472487, 3.842474614898954144, -48.12459668492483189 ) ) ;
#1841 = ADVANCED_FACE ( 'NONE', ( #1178 ), #14413, .T. ) ;
#1842 = FACE_OUTER_BOUND ( 'NONE', #5321, .T. ) ;
#1843 = EDGE_CURVE ( 'NONE', #3737, #2170, #10798, .T. ) ;
#1844 = VERTEX_POINT ( 'NONE', #10571 ) ;
#1845 = CARTESIAN_POINT ( 'NONE',  ( 58.00000000000000711, 2.256146146571122113, 38.00000000000012079 ) ) ;
#1846 = CARTESIAN_POINT ( 'NONE',  ( 45.17127246049422240, 0.000000000000000000, 33.00000000000012790 ) ) ;
#1847 = CARTESIAN_POINT ( 'NONE',  ( 12.41997800841440913, -64.16417350152465815, -3.791131921652696857 ) ) ;
#1848 = ORIENTED_EDGE ( 'NONE', *, *, #2501, .F. ) ;
#1849 = CARTESIAN_POINT ( 'NONE',  ( 61.44362764059101067, -6.606194471396438672, 48.51982618741349285 ) ) ;
#1850 = CARTESIAN_POINT ( 'NONE',  ( 95.31453344691183815, 23.25070940071369208, 139.1143251403882459 ) ) ;
#1851 = ORIENTED_EDGE ( 'NONE', *, *, #1518, .T. ) ;
#1852 = CARTESIAN_POINT ( 'NONE',  ( 30.84974339222601003, -61.21674351969437566, -3.284692946547116854 ) ) ;
#1853 =( NAMED_UNIT ( * ) PLANE_ANGLE_UNIT ( ) SI_UNIT ( $, .RADIAN. ) );
#1854 = AXIS2_PLACEMENT_3D ( 'NONE', #11866, #11937, #6259 ) ;
#1855 = CARTESIAN_POINT ( 'NONE',  ( 121.5907739023289906, -31.78146182366520378, 56.28371344025897827 ) ) ;
#1856 = EDGE_LOOP ( 'NONE', ( #14590, #12513, #2901, #14475, #594, #2880, #7996, #8140, #13898, #988 ) ) ;
#1857 = CARTESIAN_POINT ( 'NONE',  ( 8.902849800389361690, -55.58404325705457438, 2.908775817946469111 ) ) ;
#1858 = EDGE_CURVE ( 'NONE', #14011, #8692, #13111, .T. ) ;
#1859 = DIRECTION ( 'NONE',  ( -1.000000000000000000, -0.000000000000000000, -0.000000000000000000 ) ) ;
#1860 = PLANE ( 'NONE',  #8128 ) ;
#1861 = CARTESIAN_POINT ( 'NONE',  ( 31.72322230991231962, -61.42570632716525125, -2.132522520905369312 ) ) ;
#1862 = PRESENTATION_LAYER_ASSIGNMENT (  '', '', ( #7039 ) ) ;
#1863 = VERTEX_POINT ( 'NONE', #9494 ) ;
#1864 = CARTESIAN_POINT ( 'NONE',  ( 28.59326752685518258, -57.14688517103346044, -4.208364645982451968 ) ) ;
#1865 = ORIENTED_EDGE ( 'NONE', *, *, #645, .T. ) ;
#1866 = DIRECTION ( 'NONE',  ( 1.156482317317871725E-16, -1.000000000000000000, 0.000000000000000000 ) ) ;
#1867 = DIRECTION ( 'NONE',  ( -0.000000000000000000, 0.000000000000000000, -1.000000000000000000 ) ) ;
#1868 = ADVANCED_FACE ( 'NONE', ( #28 ), #1248, .F. ) ;
#1869 = ORIENTED_EDGE ( 'NONE', *, *, #4253, .T. ) ;
#1870 = DIRECTION ( 'NONE',  ( -1.051347561198064835E-16, 1.682156097916903736E-15, -1.000000000000000000 ) ) ;
#1871 = FACE_BOUND ( 'NONE', #1070, .T. ) ;
#1872 = EDGE_CURVE ( 'NONE', #1691, #14241, #5960, .T. ) ;
#1873 = ADVANCED_FACE ( 'NONE', ( #10648, #14344 ), #12017, .F. ) ;
#1874 = CARTESIAN_POINT ( 'NONE',  ( 13.15370223272280370, -65.65107448351760411, 3.408697305258708621 ) ) ;
#1875 = CYLINDRICAL_SURFACE ( 'NONE', #8063, 0.7892041907098262810 ) ;
#1876 = DIRECTION ( 'NONE',  ( 0.000000000000000000, 0.000000000000000000, -1.000000000000000000 ) ) ;
#1877 = CIRCLE ( 'NONE', #8034, 0.5000000000000004441 ) ;
#1878 = VECTOR ( 'NONE', #4733, 1000.000000000000000 ) ;
#1879 = PLANE ( 'NONE',  #6472 ) ;
#1880 = FACE_OUTER_BOUND ( 'NONE', #12072, .T. ) ;
#1881 = EDGE_CURVE ( 'NONE', #8779, #9351, #4679, .T. ) ;
#1882 = ORIENTED_EDGE ( 'NONE', *, *, #5241, .T. ) ;
#1883 = EDGE_CURVE ( 'NONE', #7515, #2307, #5845, .T. ) ;
#1884 = AXIS2_PLACEMENT_3D ( 'NONE', #7493, #14711, #482 ) ;
#1885 = DIRECTION ( 'NONE',  ( -0.000000000000000000, -0.000000000000000000, -1.000000000000000000 ) ) ;
#1886 = VERTEX_POINT ( 'NONE', #6651 ) ;
#1887 = DIRECTION ( 'NONE',  ( -0.000000000000000000, -0.000000000000000000, 1.000000000000000000 ) ) ;
#1888 = EDGE_LOOP ( 'NONE', ( #8253, #2831, #13213, #11548 ) ) ;
#1889 = CARTESIAN_POINT ( 'NONE',  ( 54.30726695196912601, -6.397170215889376621, 54.56811043785582882 ) ) ;
#1890 = DIRECTION ( 'NONE',  ( 0.000000000000000000, 0.000000000000000000, 1.000000000000000000 ) ) ;
#1891 = CIRCLE ( 'NONE', #11736, 0.9999999999999993339 ) ;
#1892 = CYLINDRICAL_SURFACE ( 'NONE', #13333, 3.999999999999999112 ) ;
#1893 = CARTESIAN_POINT ( 'NONE',  ( 35.49198652140812982, 0.000000000000000000, 139.1143251403882459 ) ) ;
#1894 = DIRECTION ( 'NONE',  ( -1.000000000000000000, 0.000000000000000000, 0.000000000000000000 ) ) ;
#1895 = ORIENTED_EDGE ( 'NONE', *, *, #14224, .T. ) ;
#1896 = CIRCLE ( 'NONE', #6811, 8.924024642120691908 ) ;
#1897 = DIRECTION ( 'NONE',  ( 0.8656763553493057595, 0.5006040828730249359, 0.000000000000000000 ) ) ;
#1898 = AXIS2_PLACEMENT_3D ( 'NONE', #12311, #6466, #14548 ) ;
#1899 = ORIENTED_EDGE ( 'NONE', *, *, #14964, .F. ) ;
#1900 = CARTESIAN_POINT ( 'NONE',  ( 62.88869237673507229, 0.3854521819929429549, 60.61639468829817190 ) ) ;
#1901 = CARTESIAN_POINT ( 'NONE',  ( 53.41380296247595538, -0.1096349785133995947, 62.84860122826521689 ) ) ;
#1902 = DIRECTION ( 'NONE',  ( -0.01745240642731254316, 0.9998476951565652415, 0.000000000000000000 ) ) ;
#1903 = CARTESIAN_POINT ( 'NONE',  ( 58.00000000000000711, -2.249290599286311032, -38.00000000000012079 ) ) ;
#1904 = AXIS2_PLACEMENT_3D ( 'NONE', #3072, #1835, #7844 ) ;
#1905 = VERTEX_POINT ( 'NONE', #3048 ) ;
#1906 = FACE_OUTER_BOUND ( 'NONE', #7243, .T. ) ;
#1907 = VERTEX_POINT ( 'NONE', #7892 ) ;
#1908 = CARTESIAN_POINT ( 'NONE',  ( 42.07846078193830408, 23.25070940071368852, -33.00000000000012790 ) ) ;
#1909 = PRODUCT ( 'Slot', 'Slot', '', ( #13321 ) ) ;
#1910 = CIRCLE ( 'NONE', #437, 11.46463184759105403 ) ;
#1911 = VERTEX_POINT ( 'NONE', #4339 ) ;
#1912 = ORIENTED_EDGE ( 'NONE', *, *, #2866, .T. ) ;
#1913 = EDGE_CURVE ( 'NONE', #12651, #13625, #1487, .T. ) ;
#1914 = CARTESIAN_POINT ( 'NONE',  ( 27.33382790127958728, -69.39711819508849544, 4.502057496415716287 ) ) ;
#1915 = CARTESIAN_POINT ( 'NONE',  ( -30.80945343098651890, -5.389243620311580329, -48.50000000000012079 ) ) ;
#1916 = CARTESIAN_POINT ( 'NONE',  ( -21.85476584171706449, 5.329050157244581420, -48.50000000000012079 ) ) ;
#1917 = CARTESIAN_POINT ( 'NONE',  ( 80.00000000000001421, -85.24929059928629727, -32.00000000000000000 ) ) ;
#1918 = VERTEX_POINT ( 'NONE', #4502 ) ;
#1919 = DIRECTION ( 'NONE',  ( 0.000000000000000000, 0.000000000000000000, 1.000000000000000000 ) ) ;
#1920 = DIRECTION ( 'NONE',  ( -2.775557561562891351E-15, 1.000000000000000000, 0.000000000000000000 ) ) ;
#1921 = CARTESIAN_POINT ( 'NONE',  ( -12.33418063572647938, -2.249290599286303927, -50.00000000000012079 ) ) ;
#1922 = CARTESIAN_POINT ( 'NONE',  ( -32.80254285330622110, -2.278009980413881141, -58.00000000000012079 ) ) ;
#1923 = CARTESIAN_POINT ( 'NONE',  ( 11.75462132594792131, -63.18892729117400364, -3.546101824478771203 ) ) ;
#1924 = ORIENTED_EDGE ( 'NONE', *, *, #3689, .F. ) ;
#1925 = CARTESIAN_POINT ( 'NONE',  ( 69.46406466716308614, -2.366909661580891999, 72.65892047407166388 ) ) ;
#1926 = CARTESIAN_POINT ( 'NONE',  ( 54.85055839958032209, 0.000000000000000000, 139.1143251403882459 ) ) ;
#1927 = ORIENTED_EDGE ( 'NONE', *, *, #12887, .F. ) ;
#1928 = EDGE_CURVE ( 'NONE', #7657, #12792, #11487, .T. ) ;
#1929 = CARTESIAN_POINT ( 'NONE',  ( 31.49298359385885959, -60.71197230342421136, -3.050751728647420613 ) ) ;
#1930 = ORIENTED_EDGE ( 'NONE', *, *, #9241, .F. ) ;
#1931 =( NAMED_UNIT ( * ) PLANE_ANGLE_UNIT ( ) SI_UNIT ( $, .RADIAN. ) );
#1932 = CARTESIAN_POINT ( 'NONE',  ( 112.9262740340969060, 23.25070940071369563, 139.1143251403882459 ) ) ;
#1933 = CYLINDRICAL_SURFACE ( 'NONE', #12594, 0.7892041907098262810 ) ;
#1934 = CARTESIAN_POINT ( 'NONE',  ( 11.55337909437054478, -53.31401535610196163, 3.970404413101017216 ) ) ;
#1935 = CARTESIAN_POINT ( 'NONE',  ( 13.77203033081066330, -67.83931925369921601, 3.638954064322520665 ) ) ;
#1936 = DIRECTION ( 'NONE',  ( 0.5394184268574535590, -0.8420378618367644341, 0.000000000000000000 ) ) ;
#1937 = VECTOR ( 'NONE', #1859, 1000.000000000000000 ) ;
#1938 = AXIS2_PLACEMENT_3D ( 'NONE', #13715, #5489, #850 ) ;
#1939 = CARTESIAN_POINT ( 'NONE',  ( -24.89252171451660445, -6.585377854361484040, -48.09696226170979827 ) ) ;
#1940 = EDGE_LOOP ( 'NONE', ( #13963, #5839, #12386, #9978 ) ) ;
#1941 = EDGE_CURVE ( 'NONE', #384, #14607, #5874, .T. ) ;
#1942 = CARTESIAN_POINT ( 'NONE',  ( 31.74929939486185404, -60.51083307721700777, 2.957531760941162435 ) ) ;
#1943 = ORIENTED_EDGE ( 'NONE', *, *, #9943, .T. ) ;
#1944 = CARTESIAN_POINT ( 'NONE',  ( 27.25618691382818781, -52.24929059928630437, -3.946674196986641903 ) ) ;
#1945 = CARTESIAN_POINT ( 'NONE',  ( 8.317129627286451665, -55.12654146333685645, 1.982842638417584791 ) ) ;
#1946 = ORIENTED_EDGE ( 'NONE', *, *, #207, .F. ) ;
#1947 = DIRECTION ( 'NONE',  ( -0.000000000000000000, -0.000000000000000000, -1.000000000000000000 ) ) ;
#1948 = DIRECTION ( 'NONE',  ( -1.000000000000000000, 0.000000000000000000, 0.000000000000000000 ) ) ;
#1949 = VECTOR ( 'NONE', #5608, 1000.000000000000000 ) ;
#1950 = AXIS2_PLACEMENT_3D ( 'NONE', #3567, #15192, #2641 ) ;
#1951 = CARTESIAN_POINT ( 'NONE',  ( 13.92771027672793061, -66.12098470289663510, 4.407543342774133066 ) ) ;
#1952 = ADVANCED_FACE ( 'NONE', ( #2039 ), #14463, .T. ) ;
#1953 = CARTESIAN_POINT ( 'NONE',  ( 10.16048094673748459, -52.84914412566558894, 3.506280953151645896 ) ) ;
#1954 = DIRECTION ( 'NONE',  ( 0.000000000000000000, -1.000000000000000000, 0.000000000000000000 ) ) ;
#1955 = FACE_OUTER_BOUND ( 'NONE', #5403, .T. ) ;
#1956 = DIRECTION ( 'NONE',  ( 0.000000000000000000, -1.000000000000000000, 0.000000000000000000 ) ) ;
#1957 = CARTESIAN_POINT ( 'NONE',  ( -16.99999999999998579, -2.249290599286303927, -50.50000000000012079 ) ) ;
#1958 = VECTOR ( 'NONE', #6701, 1000.000000000000000 ) ;
#1959 = ORIENTED_EDGE ( 'NONE', *, *, #12909, .T. ) ;
#1960 = CARTESIAN_POINT ( 'NONE',  ( 13.81529256454321519, -67.42878071148635399, -4.083908651492614617 ) ) ;
#1961 = VERTEX_POINT ( 'NONE', #13894 ) ;
#1962 = CARTESIAN_POINT ( 'NONE',  ( 32.37487573296866117, -54.69456399997503127, -3.125517714509074452 ) ) ;
#1963 = ORIENTED_EDGE ( 'NONE', *, *, #10035, .T. ) ;
#1964 = CARTESIAN_POINT ( 'NONE',  ( 28.20373290646733722, -66.75404937493291868, 3.551013195539360012 ) ) ;
#1965 = CARTESIAN_POINT ( 'NONE',  ( 51.75774672102440377, 0.000000000000000000, 139.1143251403882459 ) ) ;
#1966 = CARTESIAN_POINT ( 'NONE',  ( 80.00000000000001421, -74.24929059928631148, 4.000000000000000000 ) ) ;
#1967 = CARTESIAN_POINT ( 'NONE',  ( 20.86173033120691045, -52.24929059928630437, 0.000000000000000000 ) ) ;
#1968 = EDGE_CURVE ( 'NONE', #5446, #15191, #10679, .T. ) ;
#1969 = EDGE_CURVE ( 'NONE', #11430, #3386, #11495, .T. ) ;
#1970 = PLANE ( 'NONE',  #11844 ) ;
#1971 = ADVANCED_FACE ( 'NONE', ( #10048 ), #12232, .T. ) ;
#1972 = ORIENTED_EDGE ( 'NONE', *, *, #7774, .T. ) ;
#1973 = CARTESIAN_POINT ( 'NONE',  ( 18.24487436548682240, -53.24929059928630437, 6.492462156583986399 ) ) ;
#1974 = CARTESIAN_POINT ( 'NONE',  ( 8.871493660177725005, -54.05847863454847158, -2.186919301701681473 ) ) ;
#1975 = CARTESIAN_POINT ( 'NONE',  ( -16.99999999999998579, -2.249290599286303927, 36.00000000000012079 ) ) ;
#1976 = CARTESIAN_POINT ( 'NONE',  ( 33.38971411695204949, -58.06117555224668081, 1.821720187977000638 ) ) ;
#1977 = ADVANCED_FACE ( 'NONE', ( #4185 ), #5430, .F. ) ;
#1978 = VERTEX_POINT ( 'NONE', #9357 ) ;
#1979 = ORIENTED_EDGE ( 'NONE', *, *, #6666, .F. ) ;
#1980 = TOROIDAL_SURFACE ( 'NONE', #12070, 8.500000000000000000, 0.5000000000000000000 ) ;
#1981 = DIRECTION ( 'NONE',  ( 0.000000000000000000, 0.000000000000000000, -1.000000000000000000 ) ) ;
#1982 = ORIENTED_EDGE ( 'NONE', *, *, #1177, .F. ) ;
#1983 = CARTESIAN_POINT ( 'NONE',  ( 98.40734512546775647, 23.25070940071369208, -33.00000000000012790 ) ) ;
#1984 = ORIENTED_EDGE ( 'NONE', *, *, #471, .F. ) ;
#1985 = ORIENTED_EDGE ( 'NONE', *, *, #12699, .T. ) ;
#1986 = VECTOR ( 'NONE', #11667, 1000.000000000000000 ) ;
#1987 = CONTEXT_DEPENDENT_SHAPE_REPRESENTATION ( #10875, #2360 ) ;
#1988 = CARTESIAN_POINT ( 'NONE',  ( 10.23047706855410688, -60.71197230342353635, -3.050751728647111083 ) ) ;
#1989 = CARTESIAN_POINT ( 'NONE',  ( -24.91612020358099855, 2.875255380930533455, -48.00000000000010658 ) ) ;
#1990 = CIRCLE ( 'NONE', #12570, 0.7892041907098262810 ) ;
#1991 = CARTESIAN_POINT ( 'NONE',  ( 53.41380296247595538, -0.1096349785133995947, 60.61639468829817190 ) ) ;
#1992 = ORIENTED_EDGE ( 'NONE', *, *, #6390, .F. ) ;
#1993 = CARTESIAN_POINT ( 'NONE',  ( 20.86173033120691045, -52.24929059928630437, 0.000000000000000000 ) ) ;
#1994 = CARTESIAN_POINT ( 'NONE',  ( 14.38963276113423895, -69.39711819508849544, 4.502057496415707405 ) ) ;
#1995 = DIRECTION ( 'NONE',  ( 1.000000000000000000, 0.000000000000000000, 0.000000000000000000 ) ) ;
#1996 = CARTESIAN_POINT ( 'NONE',  ( 108.0866310645538562, 23.25070940071369563, 33.00000000000012790 ) ) ;
#1997 = FACE_OUTER_BOUND ( 'NONE', #3421, .T. ) ;
#1998 = VERTEX_POINT ( 'NONE', #6049 ) ;
#1999 = VECTOR ( 'NONE', #1490, 1000.000000000000000 ) ;
#2000 = CYLINDRICAL_SURFACE ( 'NONE', #1676, 0.5000000000000001110 ) ;
#2001 = APPLICATION_CONTEXT ( 'automotive_design' ) ;
#2002 = AXIS2_PLACEMENT_3D ( 'NONE', #5472, #5783, #13619 ) ;
#2003 = VECTOR ( 'NONE', #9083, 1000.000000000000000 ) ;
#2004 = DIRECTION ( 'NONE',  ( 0.000000000000000000, 1.000000000000000000, -0.000000000000000000 ) ) ;
#2005 = EDGE_LOOP ( 'NONE', ( #13844, #10093, #5618, #6415 ) ) ;
#2006 =( NAMED_UNIT ( * ) SI_UNIT ( $, .STERADIAN. ) SOLID_ANGLE_UNIT ( ) );
#2007 = SURFACE_STYLE_USAGE ( .BOTH. , #12559 ) ;
#2008 = DIRECTION ( 'NONE',  ( 0.000000000000000000, 0.000000000000000000, 1.000000000000000000 ) ) ;
#2009 = FACE_OUTER_BOUND ( 'NONE', #13278, .T. ) ;
#2010 = ORIENTED_EDGE ( 'NONE', *, *, #882, .F. ) ;
#2011 = DIRECTION ( 'NONE',  ( 0.4848096202550659650, 0.8746197071345572782, -0.000000000000000000 ) ) ;
#2012 = AXIS2_PLACEMENT_3D ( 'NONE', #10249, #6482, #7789 ) ;
#2013 = PRODUCT_DEFINITION_SHAPE ( 'NONE', 'NONE',  #15234 ) ;
#2014 = AXIS2_PLACEMENT_3D ( 'NONE', #10154, #15082, #14841 ) ;
#2015 = AXIS2_PLACEMENT_3D ( 'NONE', #4791, #3637, #10483 ) ;
#2016 = EDGE_CURVE ( 'NONE', #8583, #13229, #9550, .T. ) ;
#2017 = CARTESIAN_POINT ( 'NONE',  ( 0.5043391135745837195, 0.8906624217387615339, -58.00000000000012079 ) ) ;
#2018 = DIRECTION ( 'NONE',  ( 0.000000000000000000, 0.000000000000000000, -1.000000000000000000 ) ) ;
#2019 = EDGE_CURVE ( 'NONE', #8234, #7396, #8440, .T. ) ;
#2020 = VECTOR ( 'NONE', #2381, 1000.000000000000000 ) ;
#2021 = PLANE ( 'NONE',  #6174 ) ;
#2022 = CARTESIAN_POINT ( 'NONE',  ( 62.80358567007132820, -3.842053655357405173, 62.84860122826521689 ) ) ;
#2023 = EDGE_LOOP ( 'NONE', ( #2080, #1378, #2516, #4174 ) ) ;
#2024 = EDGE_LOOP ( 'NONE', ( #12450, #9299, #2404, #8022 ) ) ;
#2025 = PLANE ( 'NONE',  #9342 ) ;
#2026 = VECTOR ( 'NONE', #8584, 1000.000000000000000 ) ;
#2027 = ORIENTED_EDGE ( 'NONE', *, *, #10558, .T. ) ;
#2028 = DIRECTION ( 'NONE',  ( 0.8746197071345572782, -0.4848096202550659650, -0.000000000000000000 ) ) ;
#2029 = LINE ( 'NONE', #6722, #8175 ) ;
#2030 = EDGE_LOOP ( 'NONE', ( #2808, #10539, #4606, #9460 ) ) ;
#2031 = CARTESIAN_POINT ( 'NONE',  ( 50.01091543003727224, 0.000000000000000000, 33.00000000000012790 ) ) ;
#2032 = LINE ( 'NONE', #10277, #9994 ) ;
#2033 = AXIS2_PLACEMENT_3D ( 'NONE', #3160, #1776, #10090 ) ;
#2034 = CARTESIAN_POINT ( 'NONE',  ( 13.41074896738031264, -66.37912134691028143, 3.509717431434834722 ) ) ;
#2035 =( BOUNDED_SURFACE ( )  B_SPLINE_SURFACE ( 3, 2, ( 
 ( #4434, #9142, #13828 ),
 ( #14358, #124, #8357 ),
 ( #12029, #3800, #7266 ),
 ( #2427, #2579, #1344 ),
 ( #8504, #8435, #4808 ),
 ( #13125, #10891, #7118 ),
 ( #12976, #4888, #13047 ),
 ( #8571, #9507, #10663 ),
 ( #9437, #12115, #13194 ),
 ( #3875, #1496, #13270 ),
 ( #11804, #1574, #2719 ),
 ( #6203, #7420, #11954 ),
 ( #2653, #347, #5037 ),
 ( #6270, #7342, #271 ) ),
 .UNSPECIFIED., .F., .F., .F. ) 
 B_SPLINE_SURFACE_WITH_KNOTS ( ( 4, 2, 2, 2, 2, 2, 4 ),
 ( 3, 3 ),
 ( 0.001417163504557061859, 0.002234205688869395946, 0.002642726781025562990, 0.003051247873181730033, 0.003459768965337897077, 0.003868290057494064120, 0.004685332241806398207 ),
 ( 0.000000000000000000, 1.000000000000000000 ),
 .UNSPECIFIED. ) 
 GEOMETRIC_REPRESENTATION_ITEM ( )  RATIONAL_B_SPLINE_SURFACE ( (
 ( 1.000000000000000000, 0.7071067811865475727, 1.000000000000000000),
 ( 1.000000000000000000, 0.7218508617830416974, 1.000000000000000000),
 ( 1.000000000000000000, 0.7387008909037698912, 1.000000000000000000),
 ( 1.000000000000000000, 0.7647615808955466887, 1.000000000000000000),
 ( 1.000000000000000000, 0.7734065576773528905, 1.000000000000000000),
 ( 1.000000000000000000, 0.7903558204260753284, 1.000000000000000000),
 ( 1.000000000000000000, 0.7987454157989255510, 1.000000000000000000),
 ( 1.000000000000000000, 0.8144265709895797123, 1.000000000000000000),
 ( 1.000000000000000000, 0.8216999247151044461, 1.000000000000000000),
 ( 1.000000000000000000, 0.8348485599609545282, 1.000000000000000000),
 ( 1.000000000000000000, 0.8407795038257930287, 1.000000000000000000),
 ( 1.000000000000000000, 0.8552130772089094890, 1.000000000000000000),
 ( 1.000000000000000000, 0.8606507091654866937, 1.000000000000000000),
 ( 1.000000000000000000, 0.8606282562001421610, 1.000000000000000000) ) ) 
 REPRESENTATION_ITEM ( '' )  SURFACE ( )  );
#2036 = EDGE_CURVE ( 'NONE', #12382, #4409, #3728, .T. ) ;
#2037 = EDGE_CURVE ( 'NONE', #9017, #8990, #9439, .T. ) ;
#2038 = DIRECTION ( 'NONE',  ( -1.000000000000000000, 0.000000000000000000, 0.000000000000000000 ) ) ;
#2039 = FACE_OUTER_BOUND ( 'NONE', #12782, .T. ) ;
#2040 = CYLINDRICAL_SURFACE ( 'NONE', #3467, 10.00000000000000178 ) ;
#2041 = PRODUCT_DEFINITION_SHAPE ( 'NONE', 'NONE',  #6372 ) ;
#2042 = VECTOR ( 'NONE', #13527, 1000.000000000000000 ) ;
#2043 = DIRECTION ( 'NONE',  ( -0.9744556954135530358, 0.2245798247307378148, 0.000000000000000000 ) ) ;
#2044 = DIRECTION ( 'NONE',  ( 0.000000000000000000, 0.000000000000000000, -1.000000000000000000 ) ) ;
#2045 = AXIS2_PLACEMENT_3D ( 'NONE', #2916, #4283, #8985 ) ;
#2046 = ORIENTED_EDGE ( 'NONE', *, *, #8831, .F. ) ;
#2047 = CARTESIAN_POINT ( 'NONE',  ( 13.85081399190160667, -68.05329818779055984, -4.069437921243382661 ) ) ;
#2048 = ORIENTED_EDGE ( 'NONE', *, *, #14002, .F. ) ;
#2049 = CARTESIAN_POINT ( 'NONE',  ( -65.00000000000001421, -85.24929059928631148, 19.99999999999999645 ) ) ;
#2050 = ORIENTED_EDGE ( 'NONE', *, *, #12034, .T. ) ;
#2051 = DIRECTION ( 'NONE',  ( -0.6727821148276317276, 0.7398406760702329610, 0.000000000000000000 ) ) ;
#2052 = CARTESIAN_POINT ( 'NONE',  ( 17.75919831123052361, -66.70789582472772850, -6.276998965480669490 ) ) ;
#2053 = DIRECTION ( 'NONE',  ( -0.8746197071345569451, 0.4848096202550666312, 0.000000000000000000 ) ) ;
#2054 = DIRECTION ( 'NONE',  ( -1.000000000000000000, -0.000000000000000000, -0.000000000000000000 ) ) ;
#2055 = ORIENTED_EDGE ( 'NONE', *, *, #13611, .T. ) ;
#2056 = AXIS2_PLACEMENT_3D ( 'NONE', #14986, #11355, #816 ) ;
#2057 = DIRECTION ( 'NONE',  ( 0.000000000000000000, 0.000000000000000000, -1.000000000000000000 ) ) ;
#2058 = EDGE_CURVE ( 'NONE', #5785, #11281, #11021, .T. ) ;
#2059 = EDGE_LOOP ( 'NONE', ( #10542, #7788, #6445, #7214 ) ) ;
#2060 = DIRECTION ( 'NONE',  ( 8.659560562354330119E-17, 0.7071067811865966446, -0.7071067811864982788 ) ) ;
#2061 = CARTESIAN_POINT ( 'NONE',  ( 8.696318251036124991, -54.32767344845774460, -2.126657344578855025 ) ) ;
#2062 = CARTESIAN_POINT ( 'NONE',  ( 17.09549820959326638, -96.56299909827106376, 1.347403282660979640 ) ) ;
#2063 = EDGE_CURVE ( 'NONE', #7033, #5832, #2905, .T. ) ;
#2064 = CARTESIAN_POINT ( 'NONE',  ( 20.86173033120691045, -82.24929059928629727, 0.000000000000000000 ) ) ;
#2065 = ORIENTED_EDGE ( 'NONE', *, *, #2181, .T. ) ;
#2066 = LINE ( 'NONE', #14079, #8795 ) ;
#2067 = ORIENTED_EDGE ( 'NONE', *, *, #10207, .F. ) ;
#2068 = LINE ( 'NONE', #4686, #10105 ) ;
#2069 = ORIENTED_EDGE ( 'NONE', *, *, #8884, .T. ) ;
#2070 = CARTESIAN_POINT ( 'NONE',  ( 56.56161818778031858, -7.613266777470379942, 48.51982618741349285 ) ) ;
#2071 = CARTESIAN_POINT ( 'NONE',  ( 96.29968967959054282, 25.52935533987996664, -33.00000000000012790 ) ) ;
#2072 = EDGE_CURVE ( 'NONE', #844, #13652, #11497, .T. ) ;
#2073 = CARTESIAN_POINT ( 'NONE',  ( 114.6731053250840233, 21.75070940071369918, 139.1143251403882459 ) ) ;
#2074 = LINE ( 'NONE', #12546, #8885 ) ;
#2075 = ORIENTED_EDGE ( 'NONE', *, *, #8292, .T. ) ;
#2076 = CARTESIAN_POINT ( 'NONE',  ( 21.74884261173415467, -85.24929059928631148, -4.000000000000000888 ) ) ;
#2077 = CARTESIAN_POINT ( 'NONE',  ( 69.45172263401887847, -2.801098317861658860, 76.51381904750685692 ) ) ;
#2078 = DIRECTION ( 'NONE',  ( 0.000000000000000000, 1.000000000000000000, 0.000000000000000000 ) ) ;
#2079 = CARTESIAN_POINT ( 'NONE',  ( 23.62269406303978769, -57.98711502980034282, 6.432599168432319381 ) ) ;
#2080 = ORIENTED_EDGE ( 'NONE', *, *, #9815, .F. ) ;
#2081 = CARTESIAN_POINT ( 'NONE',  ( 64.64681977576810823, -12.79380737173441140, 82.40005259842790508 ) ) ;
#2082 = ADVANCED_FACE ( 'NONE', ( #14130 ), #2348, .T. ) ;
#2083 = EDGE_CURVE ( 'NONE', #12669, #3922, #4810, .T. ) ;
#2084 = LINE ( 'NONE', #12556, #14 ) ;
#2085 = ORIENTED_EDGE ( 'NONE', *, *, #1603, .F. ) ;
#2086 = CARTESIAN_POINT ( 'NONE',  ( 130.4454129427046496, 23.25070940071369563, -13.14990448602692474 ) ) ;
#2087 = SHAPE_REPRESENTATION_RELATIONSHIP ( 'NONE' , 'NONE' ,  #1557, #14388 ) ;
#2088 = DIRECTION ( 'NONE',  ( -0.8746197071345542806, 0.4848096202550715161, 0.000000000000000000 ) ) ;
#2089 = CARTESIAN_POINT ( 'NONE',  ( 55.86211336638498182, 2.337731330496643167, 62.84860122826521689 ) ) ;
#2090 = ORIENTED_EDGE ( 'NONE', *, *, #525, .T. ) ;
#2091 = CARTESIAN_POINT ( 'NONE',  ( -9.456839514482959785, 2.659958822950722279, -48.50000000000011369 ) ) ;
#2092 = CARTESIAN_POINT ( 'NONE',  ( -16.99999999999998579, -2.249290599286303927, 38.00000000000012079 ) ) ;
#2093 = CARTESIAN_POINT ( 'NONE',  ( 71.64423341085262109, -14.38582895075278500, 71.19766410831374515 ) ) ;
#2094 = CARTESIAN_POINT ( 'NONE',  ( 0.5043391135745837195, 0.8906624217387615339, 57.50000000000012079 ) ) ;
#2095 = CARTESIAN_POINT ( 'NONE',  ( 80.00000000000001421, -74.24929059928631148, -8.000000000000001776 ) ) ;
#2096 = ORIENTED_EDGE ( 'NONE', *, *, #9756, .F. ) ;
#2097 = ORIENTED_EDGE ( 'NONE', *, *, #7253, .F. ) ;
#2098 = VECTOR ( 'NONE', #13951, 1000.000000000000000 ) ;
#2099 = CARTESIAN_POINT ( 'NONE',  ( 112.9262740340969060, 21.75070940071369918, 33.00000000000012790 ) ) ;
#2100 = ORIENTED_EDGE ( 'NONE', *, *, #7921, .T. ) ;
#2101 = CARTESIAN_POINT ( 'NONE',  ( 8.201103799357262858, -57.48563641131178770, -1.816685854991388238 ) ) ;
#2102 = CYLINDRICAL_SURFACE ( 'NONE', #779, 4.194885682587998765 ) ;
#2103 = ORIENTED_EDGE ( 'NONE', *, *, #14824, .T. ) ;
#2105 = VERTEX_POINT ( 'NONE', #10434 ) ;
#2104 = CYLINDRICAL_SURFACE ( 'NONE', #3264, 6.484807146443463566 ) ;
#2106 = LINE ( 'NONE', #3423, #13928 ) ;
#2107 = ADVANCED_FACE ( 'NONE', ( #12826 ), #8361, .T. ) ;
#2108 = CARTESIAN_POINT ( 'NONE',  ( -7.499999999999985789, -2.249290599286303927, -47.50000000000012079 ) ) ;
#2109 = AXIS2_PLACEMENT_3D ( 'NONE', #1317, #8179, #5879 ) ;
#2110 = CARTESIAN_POINT ( 'NONE',  ( -65.00000000000001421, -85.24929059928631148, 19.99999999999999645 ) ) ;
#2111 = CARTESIAN_POINT ( 'NONE',  ( 29.67303256468918704, -52.24929059928631858, -3.113412445639874182 ) ) ;
#2112 = CARTESIAN_POINT ( 'NONE',  ( -22.16581936427349575, -2.249290599286303483, 57.50000000000012079 ) ) ;
#2113 = FACE_OUTER_BOUND ( 'NONE', #14298, .T. ) ;
#2114 = CARTESIAN_POINT ( 'NONE',  ( -25.21252699837112132, -6.998437922861944216, -48.36782213136056896 ) ) ;
#2115 = EDGE_LOOP ( 'NONE', ( #2607, #14282, #14380, #13821 ) ) ;
#2116 = CARTESIAN_POINT ( 'NONE',  ( 7.330417041869147887, -50.37435811144442255, -2.733270617041293260 ) ) ;
#2117 = EDGE_LOOP ( 'NONE', ( #3377, #9705, #678, #7452 ) ) ;
#2118 = CARTESIAN_POINT ( 'NONE',  ( 32.98173233368826374, -56.83124152802057694, -2.758380730586864171 ) ) ;
#2119 = VECTOR ( 'NONE', #2226, 1000.000000000000000 ) ;
#2120 = ORIENTED_EDGE ( 'NONE', *, *, #8390, .T. ) ;
#2121 = PRESENTATION_STYLE_ASSIGNMENT (( #12672 ) ) ;
#2122 = VECTOR ( 'NONE', #7507, 1000.000000000000000 ) ;
#2123 = EDGE_CURVE ( 'NONE', #8184, #7261, #9511, .T. ) ;
#2124 = FACE_OUTER_BOUND ( 'NONE', #9570, .T. ) ;
#2125 = ADVANCED_FACE ( 'NONE', ( #11576 ), #11734, .F. ) ;
#2126 = CARTESIAN_POINT ( 'NONE',  ( -80.00000000000001421, -74.24929059928631148, -32.99999999999999289 ) ) ;
#2127 = CARTESIAN_POINT ( 'NONE',  ( 80.00000000000001421, -74.24929059928631148, 32.99999999999999289 ) ) ;
#2128 = CIRCLE ( 'NONE', #6795, 7.000000000000000000 ) ;
#2129 =( GEOMETRIC_REPRESENTATION_CONTEXT ( 3 ) GLOBAL_UNCERTAINTY_ASSIGNED_CONTEXT ( ( #13980 ) ) GLOBAL_UNIT_ASSIGNED_CONTEXT ( ( #12561, #1931, #12718 ) ) REPRESENTATION_CONTEXT ( 'NONE', 'WORKASPACE' ) );
#2130 = DIRECTION ( 'NONE',  ( 0.000000000000000000, 0.000000000000000000, -1.000000000000000000 ) ) ;
#2131 = ORIENTED_EDGE ( 'NONE', *, *, #4198, .T. ) ;
#2132 = CIRCLE ( 'NONE', #8294, 4.000000000000000000 ) ;
#2133 = AXIS2_PLACEMENT_3D ( 'NONE', #10506, #11334, #6803 ) ;
#2134 = CARTESIAN_POINT ( 'NONE',  ( 62.00000000000001421, -2.249290599286310588, 139.1143251403882459 ) ) ;
#2135 = CARTESIAN_POINT ( 'NONE',  ( 10.22565734178488839, -53.83453582474933086, -3.481203917140358151 ) ) ;
#2136 = LINE ( 'NONE', #10378, #6711 ) ;
#2137 = CARTESIAN_POINT ( 'NONE',  ( -9.855956283963589470, -8.104443761338727015, 48.08251050686958905 ) ) ;
#2138 = ORIENTED_EDGE ( 'NONE', *, *, #11839, .F. ) ;
#2139 = FACE_OUTER_BOUND ( 'NONE', #1763, .T. ) ;
#2140 = TOROIDAL_SURFACE ( 'NONE', #3376, 2.000000000000000000, 1.000000000000000000 ) ;
#2141 = ORIENTED_EDGE ( 'NONE', *, *, #2037, .T. ) ;
#2142 = CARTESIAN_POINT ( 'NONE',  ( 65.00000000000001421, -87.24929059928631148, -19.99999999999999645 ) ) ;
#2143 = ORIENTED_EDGE ( 'NONE', *, *, #11339, .F. ) ;
#2144 = EDGE_CURVE ( 'NONE', #1115, #5061, #1035, .T. ) ;
#2145 = AXIS2_PLACEMENT_3D ( 'NONE', #5091, #2927, #9940 ) ;
#2146 = CARTESIAN_POINT ( 'NONE',  ( 8.876893811795392608, -60.07159297390013108, -1.862767969487477027 ) ) ;
#2147 = CARTESIAN_POINT ( 'NONE',  ( -23.68178719075091365, 3.790042057515504048, -47.74919337097016836 ) ) ;
#2148 = DIRECTION ( 'NONE',  ( -0.000000000000000000, -0.000000000000000000, -1.000000000000000000 ) ) ;
#2149 = CARTESIAN_POINT ( 'NONE',  ( 103.2469880950108063, 23.25070940071369208, 33.00000000000012790 ) ) ;
#2150 = ORIENTED_EDGE ( 'NONE', *, *, #3689, .T. ) ;
#2151 = DIRECTION ( 'NONE',  ( 0.000000000000000000, 1.000000000000000000, 1.927470528863120035E-16 ) ) ;
#2152 = DIRECTION ( 'NONE',  ( 0.000000000000000000, 0.000000000000000000, -1.000000000000000000 ) ) ;
#2153 = CARTESIAN_POINT ( 'NONE',  ( 80.00000000000001421, -85.24929059928629727, 32.00000000000000000 ) ) ;
#2154 = CLOSED_SHELL ( 'NONE', ( #8223, #12212, #1873, #6816, #3020, #5563, #3592, #7389, #14535, #15006, #9629 ) ) ;
#2155 = CARTESIAN_POINT ( 'NONE',  ( 52.94134894379979528, -2.395505968190773327, 60.61639468829817190 ) ) ;
#2156 = CARTESIAN_POINT ( 'NONE',  ( 33.74050986731716506, -53.52517728502748184, 2.732533236848883718 ) ) ;
#2157 = AXIS2_PLACEMENT_3D ( 'NONE', #2634, #7329, #9578 ) ;
#2158 = ORIENTED_EDGE ( 'NONE', *, *, #4168, .T. ) ;
#2159 = AXIS2_PLACEMENT_3D ( 'NONE', #5681, #12522, #8822 ) ;
#2160 = CARTESIAN_POINT ( 'NONE',  ( -25.46282903980762669, -6.565599745187292946, -47.50000000000012079 ) ) ;
#2161 = EDGE_CURVE ( 'NONE', #625, #5948, #13973, .T. ) ;
#2162 = CARTESIAN_POINT ( 'NONE',  ( 18.61871093201826355, -52.24929059928630437, 5.564967562786263144 ) ) ;
#2163 = ORIENTED_EDGE ( 'NONE', *, *, #1566, .T. ) ;
#2164 = DIRECTION ( 'NONE',  ( -0.000000000000000000, 1.000000000000000000, 1.445602896647339163E-16 ) ) ;
#2165 = DIRECTION ( 'NONE',  ( 0.000000000000000000, -0.000000000000000000, 1.000000000000000000 ) ) ;
#2166 = AXIS2_PLACEMENT_3D ( 'NONE', #7072, #3298, #8152 ) ;
#2167 = EDGE_LOOP ( 'NONE', ( #2376, #14738, #11687, #7222 ) ) ;
#2168 = DIRECTION ( 'NONE',  ( 0.000000000000000000, 0.000000000000000000, 1.000000000000000000 ) ) ;
#2169 = CARTESIAN_POINT ( 'NONE',  ( 53.81626139532630759, -96.56299909827106376, 11.78977872328355048 ) ) ;
#2170 = VERTEX_POINT ( 'NONE', #14207 ) ;
#2171 = AXIS2_PLACEMENT_3D ( 'NONE', #6969, #7197, #1108 ) ;
#2172 = CARTESIAN_POINT ( 'NONE',  ( 20.86173033120691045, -72.24929059928631148, 0.000000000000000000 ) ) ;
#2173 = CARTESIAN_POINT ( 'NONE',  ( -16.99999999999998579, -2.249290599286303927, -38.50000000000012790 ) ) ;
#2174 = EDGE_CURVE ( 'NONE', #8402, #322, #15127, .T. ) ;
#2175 = ADVANCED_FACE ( 'NONE', ( #4579 ), #8075, .F. ) ;
#2176 = DIRECTION ( 'NONE',  ( 0.1784957649143742442, 0.9839406800755992055, 8.214872995831076759E-16 ) ) ;
#2177 = CARTESIAN_POINT ( 'NONE',  ( 10.58727470799617087, -61.88944072237683969, 2.366779157396520006 ) ) ;
#2178 = DIRECTION ( 'NONE',  ( -0.000000000000000000, -0.000000000000000000, -1.000000000000000000 ) ) ;
#2179 = CARTESIAN_POINT ( 'NONE',  ( 70.26445833701072274, -4.474174595298148205, 76.19766410831374515 ) ) ;
#2180 = VERTEX_POINT ( 'NONE', #2505 ) ;
#2181 = EDGE_CURVE ( 'NONE', #9470, #5069, #5821, .T. ) ;
#2182 = VERTEX_POINT ( 'NONE', #14700 ) ;
#2183 = CARTESIAN_POINT ( 'NONE',  ( 33.12442989620986822, -59.21224831720009973, 1.832439066040439490 ) ) ;
#2184 = VECTOR ( 'NONE', #14243, 1000.000000000000000 ) ;
#2185 = ORIENTED_EDGE ( 'NONE', *, *, #780, .T. ) ;
#2186 = CARTESIAN_POINT ( 'NONE',  ( 65.00000000000001421, -85.27429059928630295, 22.50000000000000000 ) ) ;
#2187 = CARTESIAN_POINT ( 'NONE',  ( -32.80254285330622110, -2.278009980413880697, 48.00000000000012079 ) ) ;
#2188 = ORIENTED_EDGE ( 'NONE', *, *, #8807, .F. ) ;
#2189 = ORIENTED_EDGE ( 'NONE', *, *, #8041, .T. ) ;
#2190 = LINE ( 'NONE', #13651, #9161 ) ;
#2191 = CARTESIAN_POINT ( 'NONE',  ( 37.23881781239525424, 21.75070940071315562, 139.1143251403882459 ) ) ;
#2192 = CARTESIAN_POINT ( 'NONE',  ( 14.40311142432125990, -68.64054039872965518, 4.542265185091991064 ) ) ;
#2193 = AXIS2_PLACEMENT_3D ( 'NONE', #9260, #3255, #9025 ) ;
#2194 = CIRCLE ( 'NONE', #14254, 7.924024642120691908 ) ;
#2195 = DIRECTION ( 'NONE',  ( 0.000000000000000000, 0.000000000000000000, -1.000000000000000000 ) ) ;
#2196 = CARTESIAN_POINT ( 'NONE',  ( -30.80945343098651890, -5.389243620311580329, 48.00000000000012079 ) ) ;
#2197 = CARTESIAN_POINT ( 'NONE',  ( 105.5545870572953930, -1.749290599286305259, 13.14990448602692474 ) ) ;
#2198 = DIRECTION ( 'NONE',  ( 1.000000000000000000, 0.000000000000000000, 0.000000000000000000 ) ) ;
#2199 = EDGE_CURVE ( 'NONE', #612, #6287, #1439, .T. ) ;
#2200 = DIRECTION ( 'NONE',  ( -0.000000000000000000, 0.000000000000000000, -1.000000000000000000 ) ) ;
#2201 = ORIENTED_EDGE ( 'NONE', *, *, #14114, .F. ) ;
#2202 = CARTESIAN_POINT ( 'NONE',  ( -80.00000000000001421, -72.24929059928631148, 34.99999999999999289 ) ) ;
#2203 = ORIENTED_EDGE ( 'NONE', *, *, #9582, .F. ) ;
#2204 = VECTOR ( 'NONE', #4280, 1000.000000000000000 ) ;
#2205 = DIRECTION ( 'NONE',  ( -0.09874083311360634663, -0.9951131834500188678, 0.000000000000000000 ) ) ;
#2206 = AXIS2_PLACEMENT_3D ( 'NONE', #13645, #14797, #3100 ) ;
#2207 = ORIENTED_EDGE ( 'NONE', *, *, #11253, .T. ) ;
#2208 = CARTESIAN_POINT ( 'NONE',  ( 10.87361627771599260, -61.21666426766272906, -3.284656216408360585 ) ) ;
#2209 = DIRECTION ( 'NONE',  ( -0.8746197071345643836, 0.4848096202550529754, 0.000000000000000000 ) ) ;
#2210 = PLANE ( 'NONE',  #874 ) ;
#2211 = CARTESIAN_POINT ( 'NONE',  ( 19.97461805067967333, -85.24929059928631148, 6.000000000000001776 ) ) ;
#2212 = ORIENTED_EDGE ( 'NONE', *, *, #6687, .F. ) ;
#2213 = CARTESIAN_POINT ( 'NONE',  ( -3.190546569013415379, 0.8906624217387615339, -57.50000000000012079 ) ) ;
#2214 = CARTESIAN_POINT ( 'NONE',  ( 9.625495281565598304, -53.24070755262478372, -2.425727701579292628 ) ) ;
#2215 = PLANE ( 'NONE',  #10403 ) ;
#2216 = ADVANCED_FACE ( 'NONE', ( #13199 ), #4069, .F. ) ;
#2217 = EDGE_CURVE ( 'NONE', #7606, #996, #6616, .T. ) ;
#2218 = CARTESIAN_POINT ( 'NONE',  ( -9.456985518117400957, -7.172040337370347629, 47.50000001881890910 ) ) ;
#2219 = VERTEX_POINT ( 'NONE', #1845 ) ;
#2220 = DIRECTION ( 'NONE',  ( -0.000000000000000000, -1.000000000000000000, -0.000000000000000000 ) ) ;
#2221 = VERTEX_POINT ( 'NONE', #14362 ) ;
#2222 = DIRECTION ( 'NONE',  ( 0.000000000000000000, 1.000000000000000000, 0.000000000000000000 ) ) ;
#2223 = ORIENTED_EDGE ( 'NONE', *, *, #13272, .F. ) ;
#2224 = EDGE_LOOP ( 'NONE', ( #13942, #3623 ) ) ;
#2225 = AXIS2_PLACEMENT_3D ( 'NONE', #12713, #12477, #3242 ) ;
#2226 = DIRECTION ( 'NONE',  ( -1.000000000000000000, -1.156482317317870492E-16, 0.000000000000000000 ) ) ;
#2227 = PLANE ( 'NONE',  #7931 ) ;
#2228 = ORIENTED_EDGE ( 'NONE', *, *, #1236, .F. ) ;
#2229 = CARTESIAN_POINT ( 'NONE',  ( 0.9298897195970434737, -1.451567674087680837, -48.50000000000012079 ) ) ;
#2230 = CARTESIAN_POINT ( 'NONE',  ( 58.44010239582257071, -7.290881550929530164, 48.51982618741349285 ) ) ;
#2231 = ORIENTED_EDGE ( 'NONE', *, *, #2415, .T. ) ;
#2232 = EDGE_CURVE ( 'NONE', #2283, #1907, #613, .T. ) ;
#2233 = DIRECTION ( 'NONE',  ( -0.000000000000000000, -1.000000000000000000, -0.000000000000000000 ) ) ;
#2234 = CARTESIAN_POINT ( 'NONE',  ( -20.99999999999998579, -67.96969602390581144, -32.99999999999998579 ) ) ;
#2235 = FACE_OUTER_BOUND ( 'NONE', #6692, .T. ) ;
#2236 = CARTESIAN_POINT ( 'NONE',  ( 48.00000000000000000, -2.664535259100377906E-14, 33.00000000000012790 ) ) ;
#2237 = ORIENTED_EDGE ( 'NONE', *, *, #6729, .T. ) ;
#2238 = CARTESIAN_POINT ( 'NONE',  ( 69.40800899368780108, -3.479222266747031611, 72.26800456963103159 ) ) ;
#2239 = AXIS2_PLACEMENT_3D ( 'NONE', #8972, #14979, #9137 ) ;
#2240 = ORIENTED_EDGE ( 'NONE', *, *, #1611, .F. ) ;
#2241 = DIRECTION ( 'NONE',  ( -5.551115123125787632E-16, -1.000000000000000000, 0.000000000000000000 ) ) ;
#2242 = DIRECTION ( 'NONE',  ( -0.6560590289829806299, 0.7547095802293147804, 0.000000000000000000 ) ) ;
#2243 = AXIS2_PLACEMENT_3D ( 'NONE', #2970, #11412, #4108 ) ;
#2244 = AXIS2_PLACEMENT_3D ( 'NONE', #3620, #8329, #6091 ) ;
#2245 = DIRECTION ( 'NONE',  ( -0.4643268659472232773, 0.8856639100469372305, 0.000000000000000000 ) ) ;
#2246 = DIRECTION ( 'NONE',  ( 0.000000000000000000, -1.000000000000000000, -4.625929269271485914E-16 ) ) ;
#2247 = ORIENTED_EDGE ( 'NONE', *, *, #14497, .T. ) ;
#2248 = DIRECTION ( 'NONE',  ( -0.000000000000000000, -0.000000000000000000, 1.000000000000000000 ) ) ;
#2249 = DIRECTION ( 'NONE',  ( 0.000000000000000000, 0.000000000000000000, 1.000000000000000000 ) ) ;
#2250 = AXIS2_PLACEMENT_3D ( 'NONE', #13282, #11115, #4974 ) ;
#2251 = CARTESIAN_POINT ( 'NONE',  ( 9.826335989509445312, -61.28833066657258399, 2.085332803602911067 ) ) ;
#2252 = CARTESIAN_POINT ( 'NONE',  ( 35.49198652140812982, 23.25070940071368852, 33.00000000000012790 ) ) ;
#2253 = AXIS2_PLACEMENT_3D ( 'NONE', #4361, #3208, #664 ) ;
#2254 = DIRECTION ( 'NONE',  ( -0.8420378618367735379, -0.5394184268574396812, 9.357418084440779321E-16 ) ) ;
#2255 = CARTESIAN_POINT ( 'NONE',  ( 20.86173033120691045, -74.24929059928636832, 3.999999999999999112 ) ) ;
#2256 = EDGE_CURVE ( 'NONE', #117, #5924, #1680, .T. ) ;
#2257 = ORIENTED_EDGE ( 'NONE', *, *, #8938, .T. ) ;
#2258 = DIRECTION ( 'NONE',  ( 1.000000000000000000, -1.214306433183763862E-14, 0.000000000000000000 ) ) ;
#2259 = ORIENTED_EDGE ( 'NONE', *, *, #3210, .F. ) ;
#2260 = EDGE_CURVE ( 'NONE', #8536, #12694, #13705, .T. ) ;
#2261 = CARTESIAN_POINT ( 'NONE',  ( -2.688903428702175252E-15, 23.25070940071368142, 139.1143251403882459 ) ) ;
#2262 = CARTESIAN_POINT ( 'NONE',  ( 10.24650954764479494, -52.80227938113591790, 2.609359049418192633 ) ) ;
#2263 = EDGE_CURVE ( 'NONE', #3976, #1585, #10124, .T. ) ;
#2264 = ORIENTED_EDGE ( 'NONE', *, *, #8967, .F. ) ;
#2265 = AXIS2_PLACEMENT_3D ( 'NONE', #9325, #11542, #1239 ) ;
#2266 = CARTESIAN_POINT ( 'NONE',  ( -28.95977857253349796, -8.587818791446737876, 48.50000000000012079 ) ) ;
#2267 = CARTESIAN_POINT ( 'NONE',  ( -3.535822565187055400, 6.114368811827579187, -57.50000000000012079 ) ) ;
#2268 = CIRCLE ( 'NONE', #10878, 2.524999999999999467 ) ;
#2269 = AXIS2_PLACEMENT_3D ( 'NONE', #2169, #7871, #5641 ) ;
#2270 = DIRECTION ( 'NONE',  ( 0.8746197071345569451, -0.4848096202550666312, 0.000000000000000000 ) ) ;
#2271 = ADVANCED_FACE ( 'NONE', ( #14849 ), #5690, .F. ) ;
#2272 = DIRECTION ( 'NONE',  ( -0.8208219420614786266, 0.4549890321264269955, 0.3453061251629919726 ) ) ;
#2273 = DIRECTION ( 'NONE',  ( -0.000000000000000000, -0.000000000000000000, -1.000000000000000000 ) ) ;
#2274 = CARTESIAN_POINT ( 'NONE',  ( -16.99999999999998579, -2.249290599286303927, 57.50000000000012079 ) ) ;
#2275 = LINE ( 'NONE', #49, #1189 ) ;
#2276 = VECTOR ( 'NONE', #5661, 1000.000000000000000 ) ;
#2277 = CARTESIAN_POINT ( 'NONE',  ( -25.46282903980762669, -6.565599745187292946, -48.00000000000012079 ) ) ;
#2278 = AXIS2_PLACEMENT_3D ( 'NONE', #7930, #9165, #11445 ) ;
#2279 = ADVANCED_FACE ( 'NONE', ( #7007 ), #14950, .F. ) ;
#2280 = VERTEX_POINT ( 'NONE', #2234 ) ;
#2281 = CARTESIAN_POINT ( 'NONE',  ( 18.19235006501570240, -55.08889408817020694, -6.471126372656766712 ) ) ;
#2282 = AXIS2_PLACEMENT_3D ( 'NONE', #5396, #1078, #15167 ) ;
#2283 = VERTEX_POINT ( 'NONE', #1151 ) ;
#2284 = FACE_OUTER_BOUND ( 'NONE', #1531, .T. ) ;
#2285 = EDGE_LOOP ( 'NONE', ( #11883, #9864, #9691, #10059 ) ) ;
#2286 = DIRECTION ( 'NONE',  ( 0.000000000000000000, -0.000000000000000000, -1.000000000000000000 ) ) ;
#2287 = ADVANCED_FACE ( 'NONE', ( #15012 ), #11382, .T. ) ;
#2288 = VERTEX_POINT ( 'NONE', #5788 ) ;
#2289 = CARTESIAN_POINT ( 'NONE',  ( 65.43033136287209572, -11.84255085238262239, 75.82650736395967783 ) ) ;
#2290 = CARTESIAN_POINT ( 'NONE',  ( -65.00000000000001421, -85.24929059928629727, -19.99999999999999645 ) ) ;
#2291 = CARTESIAN_POINT ( 'NONE',  ( 10.00023835250150483, -61.42570632716525125, -2.132522520905374197 ) ) ;
#2292 = EDGE_CURVE ( 'NONE', #490, #10969, #9562, .T. ) ;
#2293 = VECTOR ( 'NONE', #12378, 1000.000000000000114 ) ;
#2294 = ORIENTED_EDGE ( 'NONE', *, *, #1364, .F. ) ;
#2295 = CIRCLE ( 'NONE', #14099, 0.7892041907098263920 ) ;
#2296 = DIRECTION ( 'NONE',  ( 1.000000000000000000, 0.000000000000000000, 0.000000000000000000 ) ) ;
#2297 = CARTESIAN_POINT ( 'NONE',  ( 11.74410493734513494, -52.28363178956084312, -3.029531835798758621 ) ) ;
#2298 = PLANE ( 'NONE',  #7952 ) ;
#2299 = CARTESIAN_POINT ( 'NONE',  ( -9.426221351845022411, -7.120495567271055037, 47.92899112040987575 ) ) ;
#2300 = ORIENTED_EDGE ( 'NONE', *, *, #13178, .F. ) ;
#2301 = ORIENTED_EDGE ( 'NONE', *, *, #9727, .T. ) ;
#2302 = CARTESIAN_POINT ( 'NONE',  ( 33.39134818683421457, -58.05408529505576354, 2.501672671502764178 ) ) ;
#2303 = EDGE_LOOP ( 'NONE', ( #5933, #14533, #2769, #11027 ) ) ;
#2304 = CARTESIAN_POINT ( 'NONE',  ( 9.200644618036296407, -59.06479067038043240, -2.757123406423053424 ) ) ;
#2305 = EDGE_LOOP ( 'NONE', ( #5018, #6461, #12046, #15107 ) ) ;
#2306 = AXIS2_PLACEMENT_3D ( 'NONE', #4421, #12665, #2198 ) ;
#2307 = VERTEX_POINT ( 'NONE', #15093 ) ;
#2308 = DIRECTION ( 'NONE',  ( 1.000000000000000000, 0.000000000000000000, 0.000000000000000000 ) ) ;
#2309 = FACE_OUTER_BOUND ( 'NONE', #14743, .T. ) ;
#2310 = ADVANCED_FACE ( 'NONE', ( #5628 ), #10397, .F. ) ;
#2311 = EDGE_CURVE ( 'NONE', #5234, #5320, #10285, .T. ) ;
#2312 = LINE ( 'NONE', #11690, #8406 ) ;
#2313 = CARTESIAN_POINT ( 'NONE',  ( 70.22960284859030367, -4.171102088227923943, 72.22139444149645726 ) ) ;
#2314 = VERTEX_POINT ( 'NONE', #4542 ) ;
#2315 = CARTESIAN_POINT ( 'NONE',  ( 118.0000000000000284, 23.25070940071369563, 33.00000000000012790 ) ) ;
#2316 = CARTESIAN_POINT ( 'NONE',  ( 65.33156958335074194, -11.86885053332497897, 72.68159868446096539 ) ) ;
#2317 = DIRECTION ( 'NONE',  ( 0.8746197071345572782, -0.4848096202550659650, 0.000000000000000000 ) ) ;
#2318 = CARTESIAN_POINT ( 'NONE',  ( 32.86365436560006259, -57.78392871903673012, 2.727962224263459134 ) ) ;
#2319 = ORIENTED_EDGE ( 'NONE', *, *, #3670, .F. ) ;
#2320 = CARTESIAN_POINT ( 'NONE',  ( 52.72354942432796321, 0.2729788054883388049, 60.61639468829817190 ) ) ;
#2321 = EDGE_LOOP ( 'NONE', ( #4204, #5930, #4129, #14661 ) ) ;
#2322 = DIRECTION ( 'NONE',  ( 0.000000000000000000, 0.000000000000000000, 1.000000000000000000 ) ) ;
#2323 = EDGE_CURVE ( 'NONE', #369, #4676, #10110, .T. ) ;
#2324 = EDGE_CURVE ( 'NONE', #1587, #2576, #14046, .T. ) ;
#2325 = DIRECTION ( 'NONE',  ( 0.000000000000000000, 0.000000000000000000, 1.000000000000000000 ) ) ;
#2326 = CARTESIAN_POINT ( 'NONE',  ( 109.8334623555409735, 23.25070940071369563, 139.1143251403882459 ) ) ;
#2327 = DIRECTION ( 'NONE',  ( 0.000000000000000000, 0.000000000000000000, 1.000000000000000000 ) ) ;
#2328 = ORIENTED_EDGE ( 'NONE', *, *, #13643, .T. ) ;
#2329 = PRODUCT_RELATED_PRODUCT_CATEGORY ( 'part', '', ( #13583 ) ) ;
#2330 = CARTESIAN_POINT ( 'NONE',  ( 65.00000000000001421, -85.24929059928631148, 17.50000000000000000 ) ) ;
#2331 = CARTESIAN_POINT ( 'NONE',  ( -65.00000000000001421, -85.24929059928631148, 22.52499999999999503 ) ) ;
#2332 = CARTESIAN_POINT ( 'NONE',  ( 0.9298897195970434737, -1.451567674087680837, 48.00000000000012079 ) ) ;
#2333 = CARTESIAN_POINT ( 'NONE',  ( 71.78261302649870856, -15.60588809212342554, 75.19766410831374515 ) ) ;
#2334 = CARTESIAN_POINT ( 'NONE',  ( -24.89835624542414649, -6.565460432723037698, -47.52815511422343775 ) ) ;
#2335 = DIRECTION ( 'NONE',  ( -1.000000000000000000, 0.000000000000000000, 0.000000000000000000 ) ) ;
#2336 = VERTEX_POINT ( 'NONE', #1994 ) ;
#2337 = ORIENTED_EDGE ( 'NONE', *, *, #2161, .T. ) ;
#2338 = DIRECTION ( 'NONE',  ( 0.3020115420618247892, -0.1674077314120183957, 0.9384901064608620613 ) ) ;
#2339 = B_SPLINE_CURVE_WITH_KNOTS ( 'NONE', 3,
 ( #5211, #9916, #14594, #8738, #7748, #10209, #12516, #4271, #14742, #1962, #5438, #3056, #12433, #7900, #7980, #2118, #3356, #5675 ),
 .UNSPECIFIED., .F., .F.,
 ( 4, 2, 2, 2, 2, 2, 2, 2, 4 ),
 ( 8.673617379884035472E-19, 0.0007600084067931453437, 0.001520016813586290471, 0.002280025220379426707, 0.003040033627172562727, 0.003800042033965699180, 0.004560050440758835200, 0.005320058847551972087, 0.006080067254345108106 ),
 .UNSPECIFIED. ) ;
#2340 = ORIENTED_EDGE ( 'NONE', *, *, #2851, .T. ) ;
#2341 = CARTESIAN_POINT ( 'NONE',  ( 12.36791015745245836, -52.24929059928631148, -3.199931146564426232 ) ) ;
#2342 = CARTESIAN_POINT ( 'NONE',  ( 23.47858629692699139, -53.24929059928630437, 6.492462156583989064 ) ) ;
#2343 = ORIENTED_EDGE ( 'NONE', *, *, #12258, .T. ) ;
#2344 = LINE ( 'NONE', #3502, #12602 ) ;
#2345 = CARTESIAN_POINT ( 'NONE',  ( 8.201103799357262858, -57.48563641131178770, 2.500000000000000000 ) ) ;
#2346 = CARTESIAN_POINT ( 'NONE',  ( 55.86211336638498182, 2.337731330496643167, 60.61639468829817190 ) ) ;
#2347 = DIRECTION ( 'NONE',  ( 0.000000000000000000, 0.000000000000000000, 1.000000000000000000 ) ) ;
#2348 = PLANE ( 'NONE',  #6120 ) ;
#2349 = LINE ( 'NONE', #11735, #9871 ) ;
#2350 = CARTESIAN_POINT ( 'NONE',  ( -2.016677571526633510E-15, 23.25070940071368497, 33.00000000000012790 ) ) ;
#2351 = CARTESIAN_POINT ( 'NONE',  ( 33.02714241137783802, -54.32767344845796487, 2.126657344578741338 ) ) ;
#2352 = ADVANCED_FACE ( 'NONE', ( #4623 ), #3158, .T. ) ;
#2353 = ORIENTED_EDGE ( 'NONE', *, *, #4906, .T. ) ;
#2354 = DIRECTION ( 'NONE',  ( 0.000000000000000000, -1.445602896647339410E-16, -1.000000000000000000 ) ) ;
#2355 = ADVANCED_FACE ( 'NONE', ( #12549 ), #6693, .F. ) ;
#2356 = ORIENTED_EDGE ( 'NONE', *, *, #6494, .T. ) ;
#2357 = EDGE_CURVE ( 'NONE', #2753, #3972, #8006, .T. ) ;
#2358 = CARTESIAN_POINT ( 'NONE',  ( 118.0000000000000284, 23.25070940071369563, 13.14990448602692474 ) ) ;
#2359 = ORIENTED_EDGE ( 'NONE', *, *, #13889, .T. ) ;
#2360 = PRODUCT_DEFINITION_SHAPE ( 'NONE', 'NONE',  #15235 ) ;
#2361 = VERTEX_POINT ( 'NONE', #14930 ) ;
#2362 = CARTESIAN_POINT ( 'NONE',  ( 65.06009362424826747, -11.28293442697746940, 77.00361647515762797 ) ) ;
#2363 = CARTESIAN_POINT ( 'NONE',  ( 57.92627403409715470, 23.25070940071368852, -33.00000000000012790 ) ) ;
#2364 = AXIS2_PLACEMENT_3D ( 'NONE', #9489, #11788, #3706 ) ;
#2365 = LINE ( 'NONE', #138, #12596 ) ;
#2366 = ORIENTED_EDGE ( 'NONE', *, *, #14128, .F. ) ;
#2367 = EDGE_CURVE ( 'NONE', #6435, #6563, #11574, .T. ) ;
#2368 = EDGE_CURVE ( 'NONE', #625, #7109, #1514, .T. ) ;
#2369 = CARTESIAN_POINT ( 'NONE',  ( -24.54316048551696028, -7.158540021523408292, 57.50000000000012079 ) ) ;
#2370 = DIRECTION ( 'NONE',  ( 0.3020115420618285085, -0.1674077314120178406, 0.9384901064608609511 ) ) ;
#2371 = LINE ( 'NONE', #4828, #9294 ) ;
#2372 = ORIENTED_EDGE ( 'NONE', *, *, #14612, .T. ) ;
#2373 = VERTEX_POINT ( 'NONE', #10703 ) ;
#2374 = CIRCLE ( 'NONE', #8282, 0.7892041907098270581 ) ;
#2375 = DIRECTION ( 'NONE',  ( -0.000000000000000000, 0.000000000000000000, 1.000000000000000000 ) ) ;
#2376 = ORIENTED_EDGE ( 'NONE', *, *, #12041, .F. ) ;
#2377 = CARTESIAN_POINT ( 'NONE',  ( 10.87371727018780199, -61.21674351969439698, 3.284692946547135950 ) ) ;
#2378 = VERTEX_POINT ( 'NONE', #6020 ) ;
#2379 = VERTEX_POINT ( 'NONE', #11851 ) ;
#2380 = CARTESIAN_POINT ( 'NONE',  ( 80.00000000000001421, -76.24929059928631148, 4.000000000000000000 ) ) ;
#2381 = DIRECTION ( 'NONE',  ( -1.000000000000000000, 2.312964634635742895E-17, -0.000000000000000000 ) ) ;
#2382 = EDGE_LOOP ( 'NONE', ( #1456, #9704, #14086, #14524 ) ) ;
#2383 = AXIS2_PLACEMENT_3D ( 'NONE', #1454, #516, #14670 ) ;
#2384 = DIRECTION ( 'NONE',  ( 0.8746197071345569451, -0.4848096202550666312, 0.000000000000000000 ) ) ;
#2385 = AXIS2_PLACEMENT_3D ( 'NONE', #14289, #10909, #11971 ) ;
#2386 = LINE ( 'NONE', #2545, #9150 ) ;
#2387 = ORIENTED_EDGE ( 'NONE', *, *, #11240, .F. ) ;
#2388 = CARTESIAN_POINT ( 'NONE',  ( -25.49999999999998934, -2.249290599286303038, 38.50000000000012790 ) ) ;
#2389 = DIRECTION ( 'NONE',  ( -0.5394184268574520047, 0.8420378618367654333, 0.000000000000000000 ) ) ;
#2390 = CIRCLE ( 'NONE', #9018, 31.00000000000000000 ) ;
#2391 = DIRECTION ( 'NONE',  ( 1.000000000000000000, 0.000000000000000000, 0.000000000000000000 ) ) ;
#2392 = AXIS2_PLACEMENT_3D ( 'NONE', #11950, #4573, #7115 ) ;
#2393 = ORIENTED_EDGE ( 'NONE', *, *, #4782, .T. ) ;
#2394 = CARTESIAN_POINT ( 'NONE',  ( 69.45589098779524306, -2.735193918331309870, 71.93997759770256550 ) ) ;
#2395 = CIRCLE ( 'NONE', #2649, 8.500000000000000000 ) ;
#2396 = EDGE_CURVE ( 'NONE', #13625, #4027, #14883, .T. ) ;
#2397 = CIRCLE ( 'NONE', #651, 1.000000000000000888 ) ;
#2398 = ORIENTED_EDGE ( 'NONE', *, *, #937, .F. ) ;
#2399 = FACE_OUTER_BOUND ( 'NONE', #1241, .T. ) ;
#2400 = DIRECTION ( 'NONE',  ( 0.000000000000000000, 1.000000000000000000, 0.000000000000000000 ) ) ;
#2401 = CARTESIAN_POINT ( 'NONE',  ( 0.000000000000000000, 0.000000000000000000, 0.000000000000000000 ) ) ;
#2402 = CARTESIAN_POINT ( 'NONE',  ( -10.12835026901530178, -8.341055813471566438, -48.12459668492476084 ) ) ;
#2403 = CARTESIAN_POINT ( 'NONE',  ( -6.999999999999978684, -69.24929059928631148, 33.00000000000000711 ) ) ;
#2404 = ORIENTED_EDGE ( 'NONE', *, *, #9772, .T. ) ;
#2405 = VECTOR ( 'NONE', #14297, 1000.000000000000000 ) ;
#2406 = CARTESIAN_POINT ( 'NONE',  ( 80.00000000000001421, -76.24929059928631148, -6.000000000000000000 ) ) ;
#2407 = CARTESIAN_POINT ( 'NONE',  ( 32.32366773688528383, -59.70501925844574487, -2.784164790581364457 ) ) ;
#2408 = AXIS2_PLACEMENT_3D ( 'NONE', #6503, #11193, #642 ) ;
#2409 = AXIS2_PLACEMENT_3D ( 'NONE', #14187, #11940, #1402 ) ;
#2410 = VECTOR ( 'NONE', #3998, 1000.000000000000000 ) ;
#2411 = DIRECTION ( 'NONE',  ( 0.000000000000000000, 0.000000000000000000, 1.000000000000000000 ) ) ;
#2412 = CARTESIAN_POINT ( 'NONE',  ( 28.80923764261828524, -63.78832907041062583, 4.037694147267533396 ) ) ;
#2413 = DIRECTION ( 'NONE',  ( 0.000000000000000000, -1.000000000000000000, 0.000000000000000000 ) ) ;
#2414 = CARTESIAN_POINT ( 'NONE',  ( 32.28540069953670866, -53.39764053564380220, -3.230171433733334485 ) ) ;
#2415 = EDGE_CURVE ( 'NONE', #587, #13534, #7090, .T. ) ;
#2416 = CIRCLE ( 'NONE', #9798, 0.5000000000000004441 ) ;
#2417 = ORIENTED_EDGE ( 'NONE', *, *, #13987, .F. ) ;
#2418 = B_SPLINE_CURVE_WITH_KNOTS ( 'NONE', 3,
 ( #4851, #9560, #4781, #14244, #8400, #10781, #7160, #10625, #9476, #11775 ),
 .UNSPECIFIED., .F., .F.,
 ( 4, 2, 2, 2, 4 ),
 ( 0.000000000000000000, 0.0003835113287520873016, 0.0007670226575041746032, 0.001150533986256262013, 0.001534045315008349206 ),
 .UNSPECIFIED. ) ;
#2419 = DIRECTION ( 'NONE',  ( -0.000000000000000000, 1.000000000000000000, 1.445602896647339163E-16 ) ) ;
#2420 = ORIENTED_EDGE ( 'NONE', *, *, #3031, .F. ) ;
#2421 = CARTESIAN_POINT ( 'NONE',  ( 8.234143183932166821, -55.39494951565961856, -1.945583896730202378 ) ) ;
#2422 = DIRECTION ( 'NONE',  ( -0.000000000000000000, -0.000000000000000000, -1.000000000000000000 ) ) ;
#2423 = AXIS2_PLACEMENT_3D ( 'NONE', #10552, #13856, #9169 ) ;
#2424 = ORIENTED_EDGE ( 'NONE', *, *, #1386, .F. ) ;
#2425 = FACE_OUTER_BOUND ( 'NONE', #6698, .T. ) ;
#2426 = CARTESIAN_POINT ( 'NONE',  ( 46.91810375148135392, 23.25070940071368852, 139.1143251403882459 ) ) ;
#2427 = CARTESIAN_POINT ( 'NONE',  ( 69.40245686127688884, -3.447530338075270429, 77.00271947736730738 ) ) ;
#2428 = CARTESIAN_POINT ( 'NONE',  ( 88.00000000000001421, 10.75070940071369208, 139.1143251403882459 ) ) ;
#2429 = DIRECTION ( 'NONE',  ( 0.000000000000000000, 0.000000000000000000, -1.000000000000000000 ) ) ;
#2430 = EDGE_CURVE ( 'NONE', #13978, #7020, #2418, .T. ) ;
#2431 = CARTESIAN_POINT ( 'NONE',  ( 14.10690393411112531, -69.39711819508849544, 4.282389493064012953 ) ) ;
#2432 = CARTESIAN_POINT ( 'NONE',  ( 32.87864669132871143, -54.08909618700784705, 2.984935890592543828 ) ) ;
#2433 = EDGE_LOOP ( 'NONE', ( #13319, #2356, #3146, #4746 ) ) ;
#2434 = FACE_OUTER_BOUND ( 'NONE', #4508, .T. ) ;
#2435 = ORIENTED_EDGE ( 'NONE', *, *, #6409, .F. ) ;
#2436 = DIRECTION ( 'NONE',  ( 0.000000000000000000, 1.000000000000000000, 0.000000000000000000 ) ) ;
#2437 = ORIENTED_EDGE ( 'NONE', *, *, #1579, .T. ) ;
#2438 = ORIENTED_EDGE ( 'NONE', *, *, #6065, .T. ) ;
#2439 = CARTESIAN_POINT ( 'NONE',  ( 65.14189293393786784, -11.91678108959769489, 75.33440516864469316 ) ) ;
#2440 = CARTESIAN_POINT ( 'NONE',  ( -0.9277479332649583021, -2.641590149077306826, -48.50000000000012079 ) ) ;
#2441 = CARTESIAN_POINT ( 'NONE',  ( 61.18622467607353599, 2.299242679852278481, 54.56811043785582882 ) ) ;
#2442 = EDGE_CURVE ( 'NONE', #10500, #3921, #13064, .T. ) ;
#2443 = APPLICATION_CONTEXT ( 'automotive_design' ) ;
#2444 = CARTESIAN_POINT ( 'NONE',  ( 8.121007193492978615, -55.93345933723870900, 2.599599694947450246 ) ) ;
#2445 = CARTESIAN_POINT ( 'NONE',  ( -20.99999999999998579, -67.96969602390581144, -115.4621125123531442 ) ) ;
#2446 = CARTESIAN_POINT ( 'NONE',  ( 19.97461805067967333, -82.24929059928629727, 6.000000000000001776 ) ) ;
#2447 = CYLINDRICAL_SURFACE ( 'NONE', #10266, 4.194885682587998765 ) ;
#2448 = VECTOR ( 'NONE', #4796, 1000.000000000000000 ) ;
#2449 = SHAPE_REPRESENTATION ( 'Small Aluminum Top-Plate Insert', ( #6315 ), #2129 ) ;
#2450 = AXIS2_PLACEMENT_3D ( 'NONE', #9013, #15022, #3321 ) ;
#2451 = ORIENTED_EDGE ( 'NONE', *, *, #6579, .T. ) ;
#2452 = LINE ( 'NONE', #6073, #12452 ) ;
#2453 = EDGE_CURVE ( 'NONE', #1998, #13307, #7412, .T. ) ;
#2454 = ORIENTED_EDGE ( 'NONE', *, *, #10449, .F. ) ;
#2455 = ORIENTED_EDGE ( 'NONE', *, *, #8388, .T. ) ;
#2456 = CARTESIAN_POINT ( 'NONE',  ( 28.56975842969000823, -65.65107448352046049, 3.408697305255369514 ) ) ;
#2457 = ORIENTED_EDGE ( 'NONE', *, *, #4253, .F. ) ;
#2458 = EDGE_CURVE ( 'NONE', #2379, #11350, #10854, .T. ) ;
#2459 = EDGE_CURVE ( 'NONE', #10521, #13525, #1232, .T. ) ;
#2460 = EDGE_CURVE ( 'NONE', #20, #6460, #4929, .T. ) ;
#2461 = CARTESIAN_POINT ( 'NONE',  ( 64.90552635791956959, 12.46743062497963450, -33.00000000000012790 ) ) ;
#2462 = LINE ( 'NONE', #7151, #2020 ) ;
#2463 = VERTEX_POINT ( 'NONE', #13163 ) ;
#2464 = VECTOR ( 'NONE', #1650, 1000.000000000000000 ) ;
#2465 = CARTESIAN_POINT ( 'NONE',  ( -80.00000000000001421, -85.24929059928629727, -32.00000000000000000 ) ) ;
#2466 = CARTESIAN_POINT ( 'NONE',  ( 69.98395955059181972, -3.185411745657274807, 73.04578369025026063 ) ) ;
#2467 = ORIENTED_EDGE ( 'NONE', *, *, #10407, .F. ) ;
#2468 = EDGE_CURVE ( 'NONE', #6074, #7994, #6913, .T. ) ;
#2469 = LINE ( 'NONE', #10702, #4099 ) ;
#2470 = FACE_OUTER_BOUND ( 'NONE', #8824, .T. ) ;
#2471 = CARTESIAN_POINT ( 'NONE',  ( 80.00000000000001421, -76.24929059928631148, 4.000000000000000000 ) ) ;
#2472 = ORIENTED_EDGE ( 'NONE', *, *, #647, .T. ) ;
#2473 = CARTESIAN_POINT ( 'NONE',  ( 65.92402464212069901, -2.249290599286308368, 47.51982618741348574 ) ) ;
#2474 = VECTOR ( 'NONE', #6981, 1000.000000000000000 ) ;
#2475 = ORIENTED_EDGE ( 'NONE', *, *, #7070, .F. ) ;
#2476 = CARTESIAN_POINT ( 'NONE',  ( 108.0866310645538562, 21.75070940071366365, -33.00000000000012790 ) ) ;
#2477 = ORIENTED_EDGE ( 'NONE', *, *, #5683, .T. ) ;
#2478 = EDGE_CURVE ( 'NONE', #7490, #5809, #14168, .T. ) ;
#2479 = CARTESIAN_POINT ( 'NONE',  ( -12.14523415828302078, -9.827631355817260328, -48.50000000000012079 ) ) ;
#2480 = DIRECTION ( 'NONE',  ( -0.000000000000000000, 0.000000000000000000, -1.000000000000000000 ) ) ;
#2481 = DIRECTION ( 'NONE',  ( -0.000000000000000000, -0.000000000000000000, 1.000000000000000000 ) ) ;
#2482 = DIRECTION ( 'NONE',  ( 0.8746197071345572782, -0.4848096202550659650, 0.000000000000000000 ) ) ;
#2483 = DIRECTION ( 'NONE',  ( 0.000000000000000000, 0.000000000000000000, -1.000000000000000000 ) ) ;
#2484 = DIRECTION ( 'NONE',  ( 0.5006040828730989878, -0.8656763553492631269, 0.000000000000000000 ) ) ;
#2485 = LINE ( 'NONE', #11874, #6953 ) ;
#2486 = CARTESIAN_POINT ( 'NONE',  ( 29.35555050496135010, -52.24929059928631148, -3.199931146564412909 ) ) ;
#2487 = AXIS2_PLACEMENT_3D ( 'NONE', #5138, #3973, #3903 ) ;
#2488 = ORIENTED_EDGE ( 'NONE', *, *, #8437, .F. ) ;
#2489 = VECTOR ( 'NONE', #2506, 1000.000000000000000 ) ;
#2490 = CARTESIAN_POINT ( 'NONE',  ( 118.5627027169299765, -35.81974489651393156, 54.40673322733725570 ) ) ;
#2491 = ORIENTED_EDGE ( 'NONE', *, *, #11907, .T. ) ;
#2492 = PLANE ( 'NONE',  #7898 ) ;
#2493 = DIRECTION ( 'NONE',  ( -0.000000000000000000, 0.000000000000000000, -1.000000000000000000 ) ) ;
#2494 = ORIENTED_EDGE ( 'NONE', *, *, #3193, .F. ) ;
#2496 = ORIENTED_EDGE ( 'NONE', *, *, #2920, .F. ) ;
#2495 = DIRECTION ( 'NONE',  ( -0.000000000000000000, 0.000000000000000000, -1.000000000000000000 ) ) ;
#2497 = CARTESIAN_POINT ( 'NONE',  ( -2.016677571526633510E-15, 23.25070940071368497, -33.00000000000012790 ) ) ;
#2498 = DIRECTION ( 'NONE',  ( 1.000000000000000000, 0.000000000000000000, 0.000000000000000000 ) ) ;
#2499 = AXIS2_PLACEMENT_3D ( 'NONE', #14059, #1204, #14138 ) ;
#2500 = CYLINDRICAL_SURFACE ( 'NONE', #12094, 0.5000000000000004441 ) ;
#2501 = EDGE_CURVE ( 'NONE', #14453, #2542, #1385, .T. ) ;
#2502 = AXIS2_PLACEMENT_3D ( 'NONE', #2, #13159, #13015 ) ;
#2503 = EDGE_CURVE ( 'NONE', #8531, #8396, #2984, .T. ) ;
#2504 = AXIS2_PLACEMENT_3D ( 'NONE', #1500, #15143, #12999 ) ;
#2505 = CARTESIAN_POINT ( 'NONE',  ( 69.46454297106444642, -2.294433322023680333, 73.19766410831374515 ) ) ;
#2506 = DIRECTION ( 'NONE',  ( 0.8746197071345572782, -0.4848096202550659650, 0.000000000000000000 ) ) ;
#2507 = FACE_OUTER_BOUND ( 'NONE', #6371, .T. ) ;
#2508 = ORIENTED_EDGE ( 'NONE', *, *, #7909, .F. ) ;
#2509 = DIRECTION ( 'NONE',  ( 0.000000000000000000, -0.000000000000000000, 1.000000000000000000 ) ) ;
#2510 = PRESENTATION_LAYER_ASSIGNMENT (  '', '', ( #11103 ) ) ;
#2511 = APPLICATION_CONTEXT ( 'automotive_design' ) ;
#2512 = CIRCLE ( 'NONE', #11105, 0.7892041907098270581 ) ;
#2513 = ORIENTED_EDGE ( 'NONE', *, *, #13184, .F. ) ;
#2514 = DIRECTION ( 'NONE',  ( 0.000000000000000000, 0.000000000000000000, -1.000000000000000000 ) ) ;
#2515 = CIRCLE ( 'NONE', #2994, 0.7892041907098261699 ) ;
#2516 = ORIENTED_EDGE ( 'NONE', *, *, #9344, .F. ) ;
#2517 = VERTEX_POINT ( 'NONE', #6249 ) ;
#2518 = CARTESIAN_POINT ( 'NONE',  ( 64.61411691698715742, -11.63232580666084104, 75.28919665560597707 ) ) ;
#2519 = DIRECTION ( 'NONE',  ( 0.000000000000000000, 0.000000000000000000, -1.000000000000000000 ) ) ;
#2520 = EDGE_CURVE ( 'NONE', #10741, #11420, #9637, .T. ) ;
#2521 = EDGE_CURVE ( 'NONE', #4675, #11128, #287, .T. ) ;
#2522 = CARTESIAN_POINT ( 'NONE',  ( 13.41466460742226019, -66.31562986446989783, -3.513916789801494911 ) ) ;
#2523 = AXIS2_PLACEMENT_3D ( 'NONE', #323, #6178, #9568 ) ;
#2524 = CARTESIAN_POINT ( 'NONE',  ( 8.741768373587657237, -56.83327624868845618, 2.758240060640735791 ) ) ;
#2525 = VECTOR ( 'NONE', #2575, 1000.000000000000000 ) ;
#2526 = AXIS2_PLACEMENT_3D ( 'NONE', #13790, #3248, #13716 ) ;
#2527 = DIRECTION ( 'NONE',  ( 0.8746197071345570562, -0.4848096202550665756, 0.000000000000000000 ) ) ;
#2528 = LINE ( 'NONE', #7217, #8314 ) ;
#2529 = VECTOR ( 'NONE', #8977, 1000.000000000000000 ) ;
#2530 = EDGE_LOOP ( 'NONE', ( #5795, #11208, #11838, #4778 ) ) ;
#2531 = ORIENTED_EDGE ( 'NONE', *, *, #242, .T. ) ;
#2532 = CARTESIAN_POINT ( 'NONE',  ( 64.33396067855510125, -11.80593389191196962, 76.20215820740455115 ) ) ;
#2533 = ORIENTED_EDGE ( 'NONE', *, *, #9628, .F. ) ;
#2534 = CARTESIAN_POINT ( 'NONE',  ( 9.488565264687794709, -59.84608319322163794, -2.809346289342996794 ) ) ;
#2535 = VERTEX_POINT ( 'NONE', #14396 ) ;
#2536 = CARTESIAN_POINT ( 'NONE',  ( 20.86173033120691045, -72.24929059928631148, -3.999999999999999112 ) ) ;
#2537 = AXIS2_PLACEMENT_3D ( 'NONE', #2266, #8277, #6963 ) ;
#2538 = EDGE_LOOP ( 'NONE', ( #7579, #9998, #4706, #1142 ) ) ;
#2539 = AXIS2_PLACEMENT_3D ( 'NONE', #13607, #14906, #3214 ) ;
#2540 = CARTESIAN_POINT ( 'NONE',  ( -21.99701278316016584, 5.237925250804929433, -48.44214661496815211 ) ) ;
#2541 = DIRECTION ( 'NONE',  ( -1.000000000000000000, 0.000000000000000000, 0.000000000000000000 ) ) ;
#2542 = VERTEX_POINT ( 'NONE', #240 ) ;
#2543 = CIRCLE ( 'NONE', #5989, 0.5000000000000004441 ) ;
#2544 = CARTESIAN_POINT ( 'NONE',  ( 0.000000000000000000, 21.75070940071363168, -33.00000000000012790 ) ) ;
#2545 = CARTESIAN_POINT ( 'NONE',  ( 55.17185982823698964, 2.720345114498381012, 62.84860122826521689 ) ) ;
#2546 = EDGE_CURVE ( 'NONE', #11391, #7994, #3838, .T. ) ;
#2547 = EDGE_LOOP ( 'NONE', ( #6515, #3993 ) ) ;
#2548 =( BOUNDED_SURFACE ( )  B_SPLINE_SURFACE ( 3, 2, ( 
 ( #12668, #13819, #9212 ),
 ( #5673, #1112, #13744 ),
 ( #4584, #3281, #2281 ),
 ( #2116, #9362, #10520 ),
 ( #808, #15133, #13899 ),
 ( #7897, #10289, #15208 ),
 ( #8054, #6892, #10361 ),
 ( #15059, #3199, #12512 ),
 ( #9287, #4664, #3353 ),
 ( #14055, #4509, #880 ),
 ( #13979, #10205, #7827 ),
 ( #1044, #1960, #5595 ),
 ( #6656, #2047, #11347 ),
 ( #11582, #5520, #4348 ) ),
 .UNSPECIFIED., .F., .F., .F. ) 
 B_SPLINE_SURFACE_WITH_KNOTS ( ( 4, 2, 2, 2, 2, 2, 4 ),
 ( 3, 3 ),
 ( 0.2948322565876038137, 0.2981287057529115603, 0.3014251549182193068, 0.3080180532488348000, 0.3146109515794502931, 0.3179074007447579842, 0.3212038499100657307 ),
 ( 0.07447800286616054755, 1.000000000000000000 ),
 .UNSPECIFIED. ) 
 GEOMETRIC_REPRESENTATION_ITEM ( )  RATIONAL_B_SPLINE_SURFACE ( (
 ( 0.9996905063672956171, 0.9979222480410725460, 1.000000000000000000),
 ( 0.9996957508213744070, 0.9979574561151137724, 1.000000000000000000),
 ( 0.9997005874846982554, 0.9979899265301206412, 1.000000000000000000),
 ( 0.9997092625818566614, 0.9980481658546502821, 1.000000000000000000),
 ( 0.9997131045178146991, 0.9980739582752989891, 1.000000000000000000),
 ( 0.9997231512649209506, 0.9981414060230869856, 1.000000000000000000),
 ( 0.9997278760137982001, 0.9981731251125871562, 1.000000000000000000),
 ( 0.9997334421747965383, 0.9982104929311652608, 1.000000000000000000),
 ( 0.9997342833619657920, 0.9982161401500547759, 1.000000000000000000),
 ( 0.9997327054743884167, 0.9982055471728220608, 1.000000000000000000),
 ( 0.9997317056072283492, 0.9981988346730122919, 1.000000000000000000),
 ( 0.9997287795965361656, 0.9981791912173640924, 1.000000000000000000),
 ( 0.9997268671536080342, 0.9981663522390450405, 1.000000000000000000),
 ( 0.9997245403443033585, 0.9981507314569679767, 1.000000000000000000) ) ) 
 REPRESENTATION_ITEM ( '' )  SURFACE ( )  );
#2549 = DIRECTION ( 'NONE',  ( 0.000000000000000000, 1.000000000000000000, -4.625929269271485914E-16 ) ) ;
#2550 = CARTESIAN_POINT ( 'NONE',  ( 0.000000000000000000, 21.75070940071312364, 33.00000000000012790 ) ) ;
#2551 = DIRECTION ( 'NONE',  ( -0.000000000000000000, -0.000000000000000000, -1.000000000000000000 ) ) ;
#2552 = EDGE_LOOP ( 'NONE', ( #8864, #11402, #9965, #6153 ) ) ;
#2553 = AXIS2_PLACEMENT_3D ( 'NONE', #10050, #14815, #4114 ) ;
#2554 = DIRECTION ( 'NONE',  ( 0.8746197071345569451, -0.4848096202550666312, 0.000000000000000000 ) ) ;
#2555 = AXIS2_PLACEMENT_3D ( 'NONE', #2155, #11535, #5712 ) ;
#2556 = ORIENTED_EDGE ( 'NONE', *, *, #6685, .T. ) ;
#2557 = DIRECTION ( 'NONE',  ( 0.3020115420618161295, -0.1674077314120152038, 0.9384901064608655030 ) ) ;
#2558 = DIRECTION ( 'NONE',  ( 0.000000000000000000, 0.000000000000000000, -1.000000000000000000 ) ) ;
#2559 = ADVANCED_FACE ( 'NONE', ( #2470 ), #12082, .F. ) ;
#2560 = ORIENTED_EDGE ( 'NONE', *, *, #9418, .T. ) ;
#2561 = CYLINDRICAL_SURFACE ( 'NONE', #3136, 1.000000000000000888 ) ;
#2562 = CARTESIAN_POINT ( 'NONE',  ( 42.07846078193830408, 0.000000000000000000, 33.00000000000012790 ) ) ;
#2563 = VERTEX_POINT ( 'NONE', #7534 ) ;
#2564 = CARTESIAN_POINT ( 'NONE',  ( -9.354272893020521451, 2.499447352334152050, -47.88483805351501132 ) ) ;
#2565 = CARTESIAN_POINT ( 'NONE',  ( 18.22133905412741228, -54.09900330348943953, 6.482993899721375186 ) ) ;
#2566 = DIRECTION ( 'NONE',  ( -0.000000000000000000, 1.000000000000000000, -0.000000000000000000 ) ) ;
#2567 = FACE_OUTER_BOUND ( 'NONE', #7297, .T. ) ;
#2568 = EDGE_CURVE ( 'NONE', #12049, #13513, #12315, .T. ) ;
#2569 = CARTESIAN_POINT ( 'NONE',  ( -24.73111225919155132, -6.857688092579577344, 47.70917337021941762 ) ) ;
#2570 = CARTESIAN_POINT ( 'NONE',  ( 30.00467404504382785, -52.27436801239488062, -4.068677752280153825 ) ) ;
#2571 = EDGE_CURVE ( 'NONE', #6801, #1961, #12080, .T. ) ;
#2572 = DIRECTION ( 'NONE',  ( 0.000000000000000000, 0.000000000000000000, -1.000000000000000000 ) ) ;
#2573 = ORIENTED_EDGE ( 'NONE', *, *, #8609, .F. ) ;
#2574 = LINE ( 'NONE', #5257, #14780 ) ;
#2575 = DIRECTION ( 'NONE',  ( 0.000000000000000000, 0.000000000000000000, -1.000000000000000000 ) ) ;
#2576 = VERTEX_POINT ( 'NONE', #8612 ) ;
#2577 = CARTESIAN_POINT ( 'NONE',  ( -65.00000000000001421, -85.24929059928631148, 17.50000000000000000 ) ) ;
#2578 = DIRECTION ( 'NONE',  ( -0.3020115420618249003, 0.1674077314120184790, -0.9384901064608621724 ) ) ;
#2579 = CARTESIAN_POINT ( 'NONE',  ( 69.36597930231356202, -3.790285738762324108, 76.23203397659162306 ) ) ;
#2580 = DIRECTION ( 'NONE',  ( 0.000000000000000000, -1.000000000000000000, -1.734723475976817547E-15 ) ) ;
#2581 = DIRECTION ( 'NONE',  ( -0.8208219420614786266, 0.4549890321264269399, 0.3453061251629920836 ) ) ;
#2582 = CARTESIAN_POINT ( 'NONE',  ( -24.73660316015754290, -6.848489080522048411, 47.70033363922482295 ) ) ;
#2583 = CARTESIAN_POINT ( 'NONE',  ( 32.96267541773152487, -54.21582538152092212, 2.947777686198818081 ) ) ;
#2584 = ORIENTED_EDGE ( 'NONE', *, *, #1928, .T. ) ;
#2585 = DIRECTION ( 'NONE',  ( 0.8656763553492972108, 0.5006040828730397019, 1.548731138869852323E-14 ) ) ;
#2586 = UNCERTAINTY_MEASURE_WITH_UNIT (LENGTH_MEASURE( 1.000000000000000082E-05 ), #3939, 'distance_accuracy_value', 'NONE');
#2587 = EDGE_CURVE ( 'NONE', #11281, #7187, #14290, .T. ) ;
#2588 = ORIENTED_EDGE ( 'NONE', *, *, #11320, .T. ) ;
#2589 = VERTEX_POINT ( 'NONE', #12224 ) ;
#2590 = CARTESIAN_POINT ( 'NONE',  ( -2.688903428702175252E-15, 23.25070940071368142, 139.1143251403882459 ) ) ;
#2591 = DIRECTION ( 'NONE',  ( 0.000000000000000000, 0.000000000000000000, -1.000000000000000000 ) ) ;
#2592 = ADVANCED_FACE ( 'NONE', ( #5299 ), #14280, .F. ) ;
#2593 = LINE ( 'NONE', #1515, #4749 ) ;
#2594 = CARTESIAN_POINT ( 'NONE',  ( 8.216359860972971774, -55.48278564389666911, 2.668166895090217761 ) ) ;
#2595 = CARTESIAN_POINT ( 'NONE',  ( -22.45192840590307881, 4.946501455397934954, 48.38495513066926890 ) ) ;
#2596 = CARTESIAN_POINT ( 'NONE',  ( -7.999999999999986677, -2.249290599286305259, -58.00000000000012079 ) ) ;
#2597 = VERTEX_POINT ( 'NONE', #12447 ) ;
#2598 = ORIENTED_EDGE ( 'NONE', *, *, #222, .T. ) ;
#2599 = ADVANCED_FACE ( 'NONE', ( #13526 ), #6308, .T. ) ;
#2600 = CARTESIAN_POINT ( 'NONE',  ( -2.016677571526633510E-15, 23.25070940071368497, -33.00000000000012790 ) ) ;
#2601 = EDGE_CURVE ( 'NONE', #14307, #7867, #11002, .T. ) ;
#2602 = ORIENTED_EDGE ( 'NONE', *, *, #6533, .T. ) ;
#2603 = CARTESIAN_POINT ( 'NONE',  ( 62.67308791069655882, 25.52935533987996664, -33.00000000000013500 ) ) ;
#2604 = ORIENTED_EDGE ( 'NONE', *, *, #9709, .F. ) ;
#2605 = CARTESIAN_POINT ( 'NONE',  ( 29.73572575534515749, -63.50313342087166291, 3.632148419033245812 ) ) ;
#2606 = AXIS2_PLACEMENT_3D ( 'NONE', #5493, #11472, #4400 ) ;
#2607 = ORIENTED_EDGE ( 'NONE', *, *, #6790, .F. ) ;
#2608 = CARTESIAN_POINT ( 'NONE',  ( 51.75774672102440377, 21.75070940071325865, 33.00000000000012790 ) ) ;
#2609 = DIRECTION ( 'NONE',  ( -0.8746197071345569451, 0.4848096202550666312, 0.000000000000000000 ) ) ;
#2610 = ORIENTED_EDGE ( 'NONE', *, *, #13697, .F. ) ;
#2611 = DIRECTION ( 'NONE',  ( 1.000000000000000000, 0.000000000000000000, 0.000000000000000000 ) ) ;
#2612 = CARTESIAN_POINT ( 'NONE',  ( -1.197457146693678753, -2.220571218158920335, -58.00000000000012079 ) ) ;
#2613 = ORIENTED_EDGE ( 'NONE', *, *, #7308, .F. ) ;
#2614 = AXIS2_PLACEMENT_3D ( 'NONE', #11749, #10212, #6899 ) ;
#2615 = CARTESIAN_POINT ( 'NONE',  ( 52.50499674461036648, -3.053107681157296582, 60.61639468829817190 ) ) ;
#2616 = DIRECTION ( 'NONE',  ( 5.551115123125786646E-16, 1.000000000000000000, 0.000000000000000000 ) ) ;
#2617 = DIRECTION ( 'NONE',  ( 0.000000000000000000, 0.000000000000000000, -1.000000000000000000 ) ) ;
#2618 = VERTEX_POINT ( 'NONE', #6600 ) ;
#2619 = ADVANCED_FACE ( 'NONE', ( #8685 ), #4134, .T. ) ;
#2620 = LINE ( 'NONE', #2776, #4621 ) ;
#2621 = EDGE_LOOP ( 'NONE', ( #4407, #5780, #6873, #3538 ) ) ;
#2622 = CARTESIAN_POINT ( 'NONE',  ( 32.48948299040029042, -60.63235088943246609, -1.938839523630887074 ) ) ;
#2623 = CARTESIAN_POINT ( 'NONE',  ( 69.37830530362853665, -3.658688429576736123, 71.30420836299177267 ) ) ;
#2624 = VECTOR ( 'NONE', #7150, 1000.000000000000000 ) ;
#2625 = EDGE_LOOP ( 'NONE', ( #838, #11779, #11928, #11061 ) ) ;
#2626 = CIRCLE ( 'NONE', #413, 4.165819364273509962 ) ;
#2627 = ORIENTED_EDGE ( 'NONE', *, *, #8772, .T. ) ;
#2628 = CYLINDRICAL_SURFACE ( 'NONE', #5345, 4.000000000000003553 ) ;
#2629 = CARTESIAN_POINT ( 'NONE',  ( 114.0000000000000284, 15.25070940071369563, -33.00000000000012790 ) ) ;
#2630 = SHAPE_REPRESENTATION ( 'Plastic-Headed Clamping Screw', ( #6315 ), #5577 ) ;
#2631 = CARTESIAN_POINT ( 'NONE',  ( -9.084028622109864060, 2.040253803610913685, -48.06338840812200175 ) ) ;
#2632 = CARTESIAN_POINT ( 'NONE',  ( 8.286643821053985448, -55.00297582946176789, 2.730999879045922896 ) ) ;
#2633 = CIRCLE ( 'NONE', #13439, 8.500000000000000000 ) ;
#2634 = CARTESIAN_POINT ( 'NONE',  ( 0.000000000000000000, 21.75070940071366365, 139.1143251403882459 ) ) ;
#2635 = CARTESIAN_POINT ( 'NONE',  ( 0.000000000000000000, 21.75070940071366365, 33.00000000000012790 ) ) ;
#2636 = CIRCLE ( 'NONE', #6196, 1.000000000000000888 ) ;
#2637 = CARTESIAN_POINT ( 'NONE',  ( -24.60511756109301373, -7.062218017875619758, 48.00656353678737531 ) ) ;
#2638 = EDGE_CURVE ( 'NONE', #11723, #4976, #458, .T. ) ;
#2639 = CARTESIAN_POINT ( 'NONE',  ( 31.29089880224823617, -53.71411213207086632, -3.559347964322167268 ) ) ;
#2640 = CIRCLE ( 'NONE', #4847, 0.7892041907098276132 ) ;
#2641 = DIRECTION ( 'NONE',  ( 0.8746197071345570562, -0.4848096202550662981, 0.000000000000000000 ) ) ;
#2642 = EDGE_LOOP ( 'NONE', ( #14948, #6854, #1726, #4839 ) ) ;
#2643 = CARTESIAN_POINT ( 'NONE',  ( 75.82472191495496361, -7.556279025088354473, 72.13615421477459222 ) ) ;
#2644 = CARTESIAN_POINT ( 'NONE',  ( 32.23491518596268435, -59.84602720838576317, -2.809343037843366364 ) ) ;
#2645 = TOROIDAL_SURFACE ( 'NONE', #11231, 7.924024642120688355, 1.000000000000000000 ) ;
#2646 = ORIENTED_EDGE ( 'NONE', *, *, #12807, .F. ) ;
#2647 = CARTESIAN_POINT ( 'NONE',  ( 20.86173033120691045, -53.24929059928630437, 0.000000000000000000 ) ) ;
#2648 = CARTESIAN_POINT ( 'NONE',  ( -5.290523468902621929, 4.522075770548486418, 57.50000000000012079 ) ) ;
#2649 = AXIS2_PLACEMENT_3D ( 'NONE', #5393, #14773, #8928 ) ;
#2650 = ADVANCED_FACE ( 'NONE', ( #9782, #524 ), #14470, .F. ) ;
#2651 = EDGE_CURVE ( 'NONE', #2283, #550, #4697, .T. ) ;
#2652 = AXIS2_PLACEMENT_3D ( 'NONE', #11078, #607, #3927 ) ;
#2653 = CARTESIAN_POINT ( 'NONE',  ( 69.46454297107186449, -2.294433320134092735, 75.47362438554114306 ) ) ;
#2654 = LINE ( 'NONE', #13195, #3969 ) ;
#2655 = CARTESIAN_POINT ( 'NONE',  ( 70.26445833701072274, -4.474174595298148205, 76.19766410831374515 ) ) ;
#2656 = EDGE_CURVE ( 'NONE', #9890, #6001, #8753, .T. ) ;
#2657 = AXIS2_PLACEMENT_3D ( 'NONE', #13816, #958, #13740 ) ;
#2658 = CARTESIAN_POINT ( 'NONE',  ( 30.30473640079415887, -52.33170319195768627, 3.962365649672984880 ) ) ;
#2659 = VECTOR ( 'NONE', #12566, 1000.000000000000000 ) ;
#2660 = ORIENTED_EDGE ( 'NONE', *, *, #1619, .T. ) ;
#2661 = CARTESIAN_POINT ( 'NONE',  ( -5.040221427466104132, 4.089237592873841365, -48.50000000000012079 ) ) ;
#2662 = ORIENTED_EDGE ( 'NONE', *, *, #6455, .F. ) ;
#2663 = CARTESIAN_POINT ( 'NONE',  ( 53.81626139532630049, -85.24929059928631148, -11.78977872328356646 ) ) ;
#2664 = VERTEX_POINT ( 'NONE', #3988 ) ;
#2666 = EDGE_LOOP ( 'NONE', ( #12457, #12075, #3735, #12990 ) ) ;
#2665 = CARTESIAN_POINT ( 'NONE',  ( -16.99999999999998579, -2.249290599286303927, -47.31370849898487307 ) ) ;
#2667 = CARTESIAN_POINT ( 'NONE',  ( 88.00000000000000000, 23.25070940071369208, 139.1143251403882459 ) ) ;
#2668 = CARTESIAN_POINT ( 'NONE',  ( 114.0000000000000284, 19.25070940071369563, 139.1143251403882459 ) ) ;
#2669 = ORIENTED_EDGE ( 'NONE', *, *, #10456, .F. ) ;
#2670 = EDGE_LOOP ( 'NONE', ( #15221, #586, #6959, #4327 ) ) ;
#2671 = ORIENTED_EDGE ( 'NONE', *, *, #6671, .F. ) ;
#2672 = EDGE_CURVE ( 'NONE', #9539, #7261, #13379, .T. ) ;
#2673 = CARTESIAN_POINT ( 'NONE',  ( -21.85476584171713199, 5.329050157244537900, 48.50000000000012079 ) ) ;
#2674 = CARTESIAN_POINT ( 'NONE',  ( 71.64423341085262109, -14.38582895075279211, 71.19766410831374515 ) ) ;
#2675 = ORIENTED_EDGE ( 'NONE', *, *, #5963, .T. ) ;
#2676 = ORIENTED_EDGE ( 'NONE', *, *, #3302, .F. ) ;
#2677 = CARTESIAN_POINT ( 'NONE',  ( -65.00000000000001421, -85.24929059928631148, 17.47499999999999787 ) ) ;
#2678 = ORIENTED_EDGE ( 'NONE', *, *, #5771, .T. ) ;
#2679 = PLANE ( 'NONE',  #2487 ) ;
#2680 = ORIENTED_EDGE ( 'NONE', *, *, #1222, .T. ) ;
#2681 = CARTESIAN_POINT ( 'NONE',  ( 29.65531183511369662, -63.62021712492886394, 2.966460067269240497 ) ) ;
#2682 = ORIENTED_EDGE ( 'NONE', *, *, #5724, .F. ) ;
#2683 = CARTESIAN_POINT ( 'NONE',  ( 23.69232253801246202, -96.56299909827106376, 4.472107801411124406 ) ) ;
#2684 = LINE ( 'NONE', #5071, #5469 ) ;
#2685 = ORIENTED_EDGE ( 'NONE', *, *, #5455, .T. ) ;
#2686 = CARTESIAN_POINT ( 'NONE',  ( 28.75670713205333229, -65.20845675887589721, -3.989712384466157058 ) ) ;
#2687 = DIRECTION ( 'NONE',  ( 1.000000000000000000, 0.000000000000000000, 0.000000000000000000 ) ) ;
#2688 = ORIENTED_EDGE ( 'NONE', *, *, #387, .T. ) ;
#2689 = ADVANCED_FACE ( 'NONE', ( #598 ), #10910, .T. ) ;
#2690 = EDGE_CURVE ( 'NONE', #10867, #12323, #8965, .T. ) ;
#2691 = AXIS2_PLACEMENT_3D ( 'NONE', #10185, #13721, #2018 ) ;
#2692 = AXIS2_PLACEMENT_3D ( 'NONE', #13877, #2254, #4722 ) ;
#2693 = CARTESIAN_POINT ( 'NONE',  ( 20.86173033120691045, -74.24929059928636832, 0.000000000000000000 ) ) ;
#2694 = DIRECTION ( 'NONE',  ( -0.000000000000000000, -0.000000000000000000, 1.000000000000000000 ) ) ;
#2695 = LINE ( 'NONE', #241, #11374 ) ;
#2696 = ORIENTED_EDGE ( 'NONE', *, *, #3785, .T. ) ;
#2697 = CARTESIAN_POINT ( 'NONE',  ( 66.24916037665502699, -11.54047404292977319, 72.19766410831375936 ) ) ;
#2698 = ORIENTED_EDGE ( 'NONE', *, *, #14591, .F. ) ;
#2699 = ORIENTED_EDGE ( 'NONE', *, *, #5308, .F. ) ;
#2700 = LINE ( 'NONE', #1552, #4226 ) ;
#2701 = AXIS2_PLACEMENT_3D ( 'NONE', #12923, #7426, #2296 ) ;
#2702 = VECTOR ( 'NONE', #7183, 1000.000000000000000 ) ;
#2703 = ORIENTED_EDGE ( 'NONE', *, *, #2920, .T. ) ;
#2704 = APPLICATION_PROTOCOL_DEFINITION ( 'draft international standard', 'automotive_design', 1998, #14245 ) ;
#2705 = CARTESIAN_POINT ( 'NONE',  ( 30.65234355186507997, 0.000000000000000000, 139.1143251403882459 ) ) ;
#2706 = DIRECTION ( 'NONE',  ( -0.000000000000000000, 0.000000000000000000, -1.000000000000000000 ) ) ;
#2707 = ADVANCED_FACE ( 'NONE', ( #11342 ), #10099, .T. ) ;
#2708 = CARTESIAN_POINT ( 'NONE',  ( -12.00298721683875236, -9.736506449376861383, -48.44214661497220931 ) ) ;
#2709 = ADVANCED_FACE ( 'NONE', ( #1955 ), #2040, .T. ) ;
#2710 = CARTESIAN_POINT ( 'NONE',  ( 18.19235006502503893, -55.08889408817012168, 6.471126372660669368 ) ) ;
#2711 = CARTESIAN_POINT ( 'NONE',  ( 58.00000000000000711, -2.249290599286309256, 87.40005259842790508 ) ) ;
#2712 = CARTESIAN_POINT ( 'NONE',  ( 29.67377849276340385, -52.24929059928631148, 3.113209168868824595 ) ) ;
#2713 = CIRCLE ( 'NONE', #3446, 0.7892041907098303888 ) ;
#2714 = CARTESIAN_POINT ( 'NONE',  ( 30.85841852505513572, -53.50006564588471036, -3.720697674323108828 ) ) ;
#2715 = CARTESIAN_POINT ( 'NONE',  ( -8.787473000605775297, 2.499856724880853864, 48.43453164808066447 ) ) ;
#2716 = EDGE_LOOP ( 'NONE', ( #102, #13483, #13190, #13571 ) ) ;
#2717 = CARTESIAN_POINT ( 'NONE',  ( 8.091875466796944139, -56.52532528994184702, -1.842181053809134994 ) ) ;
#2718 = CARTESIAN_POINT ( 'NONE',  ( 58.14816640453862107, 2.809303687574978614, 62.84860122826521689 ) ) ;
#2719 = CARTESIAN_POINT ( 'NONE',  ( 70.02887381300654113, -3.323774946711823386, 75.65470943568233508 ) ) ;
#2720 = DIRECTION ( 'NONE',  ( 0.000000000000000000, -0.000000000000000000, -1.000000000000000000 ) ) ;
#2721 = ADVANCED_FACE ( 'NONE', ( #10284 ), #1980, .T. ) ;
#2722 = DIRECTION ( 'NONE',  ( 0.000000000000000000, -1.000000000000000000, 0.000000000000000000 ) ) ;
#2723 = CARTESIAN_POINT ( 'NONE',  ( 59.93923848102027563, 1.249188229251924742, 38.50000000000012790 ) ) ;
#2724 = VECTOR ( 'NONE', #7198, 1000.000000000000000 ) ;
#2725 = EDGE_CURVE ( 'NONE', #4463, #10987, #10341, .T. ) ;
#2726 = ORIENTED_EDGE ( 'NONE', *, *, #6143, .T. ) ;
#2727 = ADVANCED_FACE ( 'NONE', ( #802, #13895 ), #5587, .T. ) ;
#2728 = CARTESIAN_POINT ( 'NONE',  ( 34.91294709002737306, -47.87885576610680971, -2.732387392806885806 ) ) ;
#2729 = UNCERTAINTY_MEASURE_WITH_UNIT (LENGTH_MEASURE( 1.000000000000000082E-05 ), #6118, 'distance_accuracy_value', 'NONE');
#2730 = ORIENTED_EDGE ( 'NONE', *, *, #5696, .T. ) ;
#2731 = DIRECTION ( 'NONE',  ( -0.000000000000000000, 1.000000000000000000, 1.445602896647339163E-16 ) ) ;
#2732 = DIRECTION ( 'NONE',  ( 0.000000000000000000, 1.000000000000000000, -0.000000000000000000 ) ) ;
#2733 = PRODUCT_DEFINITION_SHAPE ( 'NONE', 'NONE',  #15233 ) ;
#2734 = ORIENTED_EDGE ( 'NONE', *, *, #1130, .F. ) ;
#2735 = TOROIDAL_SURFACE ( 'NONE', #11317, 8.500000000000000000, 0.5000000000000000000 ) ;
#2737 = ORIENTED_EDGE ( 'NONE', *, *, #5225, .T. ) ;
#2736 = CARTESIAN_POINT ( 'NONE',  ( -11.54807159409575235, -9.445082653969818054, 48.38495513067856280 ) ) ;
#2738 = DIRECTION ( 'NONE',  ( -0.000000000000000000, -0.000000000000000000, -1.000000000000000000 ) ) ;
#2739 = EDGE_CURVE ( 'NONE', #10002, #9843, #3218, .T. ) ;
#2740 = AXIS2_PLACEMENT_3D ( 'NONE', #2346, #12658, #2270 ) ;
#2741 = EDGE_CURVE ( 'NONE', #1838, #6910, #12749, .T. ) ;
#2742 = AXIS2_PLACEMENT_3D ( 'NONE', #12942, #12000, #10937 ) ;
#2743 = FACE_OUTER_BOUND ( 'NONE', #156, .T. ) ;
#2744 = DIRECTION ( 'NONE',  ( 0.000000000000000000, 1.734723475976817547E-15, -1.000000000000000000 ) ) ;
#2745 = EDGE_CURVE ( 'NONE', #10066, #14864, #10201, .T. ) ;
#2746 = DIRECTION ( 'NONE',  ( -1.000000000000000000, 2.312964634635742895E-17, -0.000000000000000000 ) ) ;
#2747 = COLOUR_RGB ( '',0.7921568627450980005, 0.8196078431372548767, 0.9333333333333333481 ) ;
#2748 = VECTOR ( 'NONE', #8244, 1000.000000000000000 ) ;
#2749 = CARTESIAN_POINT ( 'NONE',  ( 58.00000000000000711, -2.249290599286311032, 36.00000000000012079 ) ) ;
#2750 = EDGE_CURVE ( 'NONE', #11132, #5929, #9048, .T. ) ;
#2751 = ORIENTED_EDGE ( 'NONE', *, *, #10179, .F. ) ;
#2752 = VECTOR ( 'NONE', #13088, 1000.000000000000000 ) ;
#2753 = VERTEX_POINT ( 'NONE', #5431 ) ;
#2754 = EDGE_CURVE ( 'NONE', #10773, #4753, #11577, .T. ) ;
#2755 = DIRECTION ( 'NONE',  ( 0.000000000000000000, 0.000000000000000000, -1.000000000000000000 ) ) ;
#2756 = VERTEX_POINT ( 'NONE', #1036 ) ;
#2757 = ORIENTED_EDGE ( 'NONE', *, *, #8397, .F. ) ;
#2758 = CARTESIAN_POINT ( 'NONE',  ( 29.35555050496136431, -53.24929059928631148, 3.199931146564425788 ) ) ;
#2759 = ORIENTED_EDGE ( 'NONE', *, *, #14867, .T. ) ;
#2760 = CARTESIAN_POINT ( 'NONE',  ( 28.23010146221949768, -64.93526722763043324, 4.251815205946187781 ) ) ;
#2761 = ORIENTED_EDGE ( 'NONE', *, *, #6621, .F. ) ;
#2762 = AXIS2_PLACEMENT_3D ( 'NONE', #16, #11860, #1001 ) ;
#2763 = DIRECTION ( 'NONE',  ( 1.051347561198064835E-16, 0.000000000000000000, 1.000000000000000000 ) ) ;
#2764 = CARTESIAN_POINT ( 'NONE',  ( 67.21328690825531282, 25.52935533987996664, 33.00000000000012790 ) ) ;
#2765 = ORIENTED_EDGE ( 'NONE', *, *, #1326, .T. ) ;
#2766 = VECTOR ( 'NONE', #14999, 1000.000000000000000 ) ;
#2767 = CIRCLE ( 'NONE', #11596, 10.46463184759104692 ) ;
#2768 = CARTESIAN_POINT ( 'NONE',  ( 28.33202942550260417, -66.31583591551820689, -4.137138225905601985 ) ) ;
#2769 = ORIENTED_EDGE ( 'NONE', *, *, #10207, .T. ) ;
#2770 = VECTOR ( 'NONE', #12842, 999.9999999999998863 ) ;
#2771 = CARTESIAN_POINT ( 'NONE',  ( -25.15752072101212278, 2.619472661158555038, 48.00000000000012079 ) ) ;
#2772 = CARTESIAN_POINT ( 'NONE',  ( -9.037775043065352065, 2.932694901963889489, -57.50000000000012079 ) ) ;
#2773 = DIRECTION ( 'NONE',  ( 0.5006040828730242698, -0.8656763553493063146, 0.000000000000000000 ) ) ;
#2774 = EDGE_LOOP ( 'NONE', ( #11180, #3664, #14998, #5633 ) ) ;
#2775 = AXIS2_PLACEMENT_3D ( 'NONE', #14477, #3923, #8618 ) ;
#2776 = CARTESIAN_POINT ( 'NONE',  ( 45.17127246049422240, 23.25070940071368852, 139.1143251403882459 ) ) ;
#2777 = ORIENTED_EDGE ( 'NONE', *, *, #2458, .F. ) ;
#2778 = ORIENTED_EDGE ( 'NONE', *, *, #7068, .F. ) ;
#2779 = EDGE_CURVE ( 'NONE', #6596, #3976, #7893, .T. ) ;
#2780 = CIRCLE ( 'NONE', #12865, 1.000000000000001332 ) ;
#2781 = CARTESIAN_POINT ( 'NONE',  ( -80.00000000000001421, -87.24929059928629727, 0.000000000000000000 ) ) ;
#2782 = ITEM_DEFINED_TRANSFORMATION ( 'NONE', 'NONE', #6080,  #6315 ) ;
#2783 = FACE_OUTER_BOUND ( 'NONE', #2224, .T. ) ;
#2784 = DIRECTION ( 'NONE',  ( -0.8746197071345569451, 0.4848096202550666312, 0.000000000000000000 ) ) ;
#2785 = CARTESIAN_POINT ( 'NONE',  ( 68.02719294894561131, -7.807454411681058026, 77.19766410831374515 ) ) ;
#2786 = EDGE_LOOP ( 'NONE', ( #13073, #9483, #7592, #3260 ) ) ;
#2787 = CARTESIAN_POINT ( 'NONE',  ( 7.328728967433968400, -50.37334675436643749, 2.732818608233515079 ) ) ;
#2788 = CIRCLE ( 'NONE', #14343, 9.000000000000001776 ) ;
#2789 = DIRECTION ( 'NONE',  ( -0.000000000000000000, -0.000000000000000000, -1.000000000000000000 ) ) ;
#2790 = AXIS2_PLACEMENT_3D ( 'NONE', #9319, #842, #14014 ) ;
#2791 = CARTESIAN_POINT ( 'NONE',  ( 32.46725937536812268, -53.58811172139414936, 2.311880426527626486 ) ) ;
#2792 = CARTESIAN_POINT ( 'NONE',  ( 14.31939787081870286, -67.79239290436674992, -4.531617596073229670 ) ) ;
#2793 = EDGE_CURVE ( 'NONE', #10204, #6843, #7404, .T. ) ;
#2794 = LINE ( 'NONE', #12329, #9851 ) ;
#2795 = ADVANCED_FACE ( 'NONE', ( #11496 ), #13974, .T. ) ;
#2796 = ORIENTED_EDGE ( 'NONE', *, *, #3559, .F. ) ;
#2797 = PRODUCT_RELATED_PRODUCT_CATEGORY ( 'part', '', ( #1909 ) ) ;
#2798 = CARTESIAN_POINT ( 'NONE',  ( -16.99999999999998579, -2.249290599286303927, 50.50000000000012079 ) ) ;
#2799 = LINE ( 'NONE', #7492, #3177 ) ;
#2800 = CARTESIAN_POINT ( 'NONE',  ( -5.040221427466046400, 4.089237592873870675, -48.50000000000012079 ) ) ;
#2801 = DIRECTION ( 'NONE',  ( -0.000000000000000000, -0.000000000000000000, -1.000000000000000000 ) ) ;
#2802 = VECTOR ( 'NONE', #9849, 1000.000000000000000 ) ;
#2803 = CARTESIAN_POINT ( 'NONE',  ( 12.03298173962126683, -53.28399145779480506, 4.141535524925028078 ) ) ;
#2804 = CARTESIAN_POINT ( 'NONE',  ( 80.00000000000001421, -76.24929059928631148, 6.000000000000000000 ) ) ;
#2805 =( REPRESENTATION_RELATIONSHIP ('NONE','NONE', #15125, #11972 ) REPRESENTATION_RELATIONSHIP_WITH_TRANSFORMATION ( #6529 )SHAPE_REPRESENTATION_RELATIONSHIP( ) );
#2806 = DIRECTION ( 'NONE',  ( 1.000000000000000000, -3.565820478396769525E-15, 0.000000000000000000 ) ) ;
#2807 = CARTESIAN_POINT ( 'NONE',  ( 8.464703746082088642, -58.62940108252796279, -2.501915095525329757 ) ) ;
#2808 = ORIENTED_EDGE ( 'NONE', *, *, #13184, .T. ) ;
#2809 = CYLINDRICAL_SURFACE ( 'NONE', #1473, 9.000000000000001776 ) ;
#2810 = ORIENTED_EDGE ( 'NONE', *, *, #6638, .T. ) ;
#2811 = CARTESIAN_POINT ( 'NONE',  ( 18.61871093201826000, -52.24929059928630437, 5.564967562786272914 ) ) ;
#2812 = LINE ( 'NONE', #14439, #54 ) ;
#2813 = ORIENTED_EDGE ( 'NONE', *, *, #12339, .T. ) ;
#2814 = CARTESIAN_POINT ( 'NONE',  ( 82.49066175147797253, 23.25070940071369208, -33.00000000000012790 ) ) ;
#2815 = DIRECTION ( 'NONE',  ( -1.000000000000000000, -8.673617379884035472E-17, 0.000000000000000000 ) ) ;
#2816 = CARTESIAN_POINT ( 'NONE',  ( 112.9262740340969060, 0.000000000000000000, -13.14990448602693007 ) ) ;
#2817 = CARTESIAN_POINT ( 'NONE',  ( 11.08978525922602465, -53.42148821037783790, 3.802824752091033211 ) ) ;
#2818 = LINE ( 'NONE', #10981, #1299 ) ;
#2819 = PLANE ( 'NONE',  #15180 ) ;
#2820 = EDGE_CURVE ( 'NONE', #6214, #8236, #15052, .T. ) ;
#2821 = ORIENTED_EDGE ( 'NONE', *, *, #4449, .F. ) ;
#2822 = ORIENTED_EDGE ( 'NONE', *, *, #284, .T. ) ;
#2823 = FACE_OUTER_BOUND ( 'NONE', #6199, .T. ) ;
#2824 = VERTEX_POINT ( 'NONE', #3348 ) ;
#2825 = FACE_OUTER_BOUND ( 'NONE', #8689, .T. ) ;
#2826 = ORIENTED_EDGE ( 'NONE', *, *, #8884, .F. ) ;
#2827 = CYLINDRICAL_SURFACE ( 'NONE', #13768, 0.9999999999999957812 ) ;
#2828 = ORIENTED_EDGE ( 'NONE', *, *, #10543, .F. ) ;
#2829 = CARTESIAN_POINT ( 'NONE',  ( 58.00000000000000711, 2.256146146571122113, 36.00000000000012079 ) ) ;
#2830 = CARTESIAN_POINT ( 'NONE',  ( 52.42117158417902800, -3.175556148104785148, 60.61639468829817190 ) ) ;
#2831 = ORIENTED_EDGE ( 'NONE', *, *, #1296, .F. ) ;
#2832 = ADVANCED_FACE ( 'NONE', ( #8048 ), #15128, .T. ) ;
#2833 = ADVANCED_FACE ( 'NONE', ( #4811 ), #15216, .F. ) ;
#2834 = CARTESIAN_POINT ( 'NONE',  ( -32.80254285330626374, -2.278009980413908231, -48.50000000000012079 ) ) ;
#2835 = ORIENTED_EDGE ( 'NONE', *, *, #8, .T. ) ;
#2836 = FACE_OUTER_BOUND ( 'NONE', #9540, .T. ) ;
#2837 = LINE ( 'NONE', #526, #13848 ) ;
#2838 = ORIENTED_EDGE ( 'NONE', *, *, #13570, .T. ) ;
#2839 = VECTOR ( 'NONE', #1697, 1000.000000000000000 ) ;
#2840 = CARTESIAN_POINT ( 'NONE',  ( 114.6731053250840233, 21.75070940071369918, 33.00000000000012790 ) ) ;
#2841 = ORIENTED_EDGE ( 'NONE', *, *, #7619, .F. ) ;
#2842 = ORIENTED_EDGE ( 'NONE', *, *, #7726, .T. ) ;
#2843 = DIRECTION ( 'NONE',  ( 0.000000000000000000, 1.000000000000000000, -0.000000000000000000 ) ) ;
#2844 = PLANE ( 'NONE',  #12726 ) ;
#2845 = FACE_OUTER_BOUND ( 'NONE', #7939, .T. ) ;
#2846 = DIRECTION ( 'NONE',  ( -0.000000000000000000, 0.000000000000000000, -1.000000000000000000 ) ) ;
#2847 = VECTOR ( 'NONE', #17, 1000.000000000000000 ) ;
#2848 = CARTESIAN_POINT ( 'NONE',  ( 8.858401005300839515, -57.78267463917103441, 2.727521282215370935 ) ) ;
#2849 = FACE_OUTER_BOUND ( 'NONE', #9522, .T. ) ;
#2850 = CARTESIAN_POINT ( 'NONE',  ( -10.14179456814604130, -8.352437357651758987, -48.12676452506694602 ) ) ;
#2851 = EDGE_CURVE ( 'NONE', #6117, #10912, #10666, .T. ) ;
#2852 = CARTESIAN_POINT ( 'NONE',  ( 104.0000000000000426, 11.25070940071369563, -33.00000000000014211 ) ) ;
#2853 = DIRECTION ( 'NONE',  ( -0.000000000000000000, -0.000000000000000000, -1.000000000000000000 ) ) ;
#2854 = AXIS2_PLACEMENT_3D ( 'NONE', #3382, #4535, #8079 ) ;
#2855 = CIRCLE ( 'NONE', #12962, 7.000000000000000000 ) ;
#2856 = DIRECTION ( 'NONE',  ( -1.000000000000000000, 0.000000000000000000, 0.000000000000000000 ) ) ;
#2857 = ORIENTED_EDGE ( 'NONE', *, *, #2851, .F. ) ;
#2858 = CARTESIAN_POINT ( 'NONE',  ( 20.86173033120691045, -82.24929059928629727, 0.000000000000000000 ) ) ;
#2859 = CARTESIAN_POINT ( 'NONE',  ( 8.201103799357262858, -57.48563641131178770, -1.816685854991388238 ) ) ;
#2860 = DIRECTION ( 'NONE',  ( 0.000000000000000000, 0.000000000000000000, 1.000000000000000000 ) ) ;
#2861 = AXIS2_PLACEMENT_3D ( 'NONE', #9230, #2375, #4530 ) ;
#2862 = DIRECTION ( 'NONE',  ( -0.000000000000000000, -0.000000000000000000, -1.000000000000000000 ) ) ;
#2863 =( LENGTH_UNIT ( ) NAMED_UNIT ( * ) SI_UNIT ( .MILLI., .METRE. ) );
#2864 = CIRCLE ( 'NONE', #4845, 3.000000000000000888 ) ;
#2865 = CIRCLE ( 'NONE', #5089, 11.46463184759104870 ) ;
#2866 = EDGE_CURVE ( 'NONE', #3904, #14153, #13128, .T. ) ;
#2867 = PLANE ( 'NONE',  #10844 ) ;
#2868 = EDGE_CURVE ( 'NONE', #13763, #13591, #35, .T. ) ;
#2869 = DIRECTION ( 'NONE',  ( 1.000000000000000000, 8.673617379884035472E-17, 0.000000000000000000 ) ) ;
#2870 = CARTESIAN_POINT ( 'NONE',  ( -24.91597137788995298, -6.538835002183793321, -48.06338840812244939 ) ) ;
#2871 = TOROIDAL_SURFACE ( 'NONE', #3365, 6.000000000000000000, 1.000000000000000000 ) ;
#2872 = CARTESIAN_POINT ( 'NONE',  ( 103.2469880950108063, 21.75070940071363168, -33.00000000000012790 ) ) ;
#2873 = ORIENTED_EDGE ( 'NONE', *, *, #9606, .T. ) ;
#2874 = CARTESIAN_POINT ( 'NONE',  ( -16.99999999999998579, -2.249290599286303927, -58.00000000000012079 ) ) ;
#2875 = AXIS2_PLACEMENT_3D ( 'NONE', #1034, #14047, #14970 ) ;
#2876 = ORIENTED_EDGE ( 'NONE', *, *, #7691, .F. ) ;
#2877 = CARTESIAN_POINT ( 'NONE',  ( 58.00000000000000711, 7.750709400713694741, 33.00000000000012790 ) ) ;
#2878 = DIRECTION ( 'NONE',  ( 0.8746197071345573892, -0.4848096202550657430, 0.000000000000000000 ) ) ;
#2879 = AXIS2_PLACEMENT_3D ( 'NONE', #6550, #9814, #10100 ) ;
#2880 = ORIENTED_EDGE ( 'NONE', *, *, #9276, .T. ) ;
#2881 = LINE ( 'NONE', #13499, #6694 ) ;
#2882 = CARTESIAN_POINT ( 'NONE',  ( 13.95756414556647762, -69.39711819508849544, -4.056575093033447210 ) ) ;
#2883 = EDGE_LOOP ( 'NONE', ( #10438, #4917, #8801, #2841 ) ) ;
#2884 = CYLINDRICAL_SURFACE ( 'NONE', #6464, 1.000000000000000888 ) ;
#2885 = AXIS2_PLACEMENT_3D ( 'NONE', #3967, #504, #14517 ) ;
#2886 = EDGE_CURVE ( 'NONE', #8619, #3132, #2349, .T. ) ;
#2887 = VERTEX_POINT ( 'NONE', #8441 ) ;
#2888 = CARTESIAN_POINT ( 'NONE',  ( 11.71878661736996108, -52.27436801240079944, 4.068677752283970328 ) ) ;
#2889 = PRODUCT ( 'Plastic-Headed Retaining Pin', 'Plastic-Headed Retaining Pin', '', ( #4939 ) ) ;
#2890 = CIRCLE ( 'NONE', #11989, 0.9999999999999965583 ) ;
#2891 = AXIS2_PLACEMENT_3D ( 'NONE', #5109, #14495, #8637 ) ;
#2892 = DIRECTION ( 'NONE',  ( 1.000000000000000000, 0.000000000000000000, 0.000000000000000000 ) ) ;
#2893 = CARTESIAN_POINT ( 'NONE',  ( 58.00000000000000711, -2.249290599286311032, -49.31370849898490150 ) ) ;
#2894 = ORIENTED_EDGE ( 'NONE', *, *, #4315, .T. ) ;
#2895 = VERTEX_POINT ( 'NONE', #5904 ) ;
#2896 = CARTESIAN_POINT ( 'NONE',  ( 10.00023835250150483, -61.42570632716525125, 2.132522520905368868 ) ) ;
#2897 = EDGE_LOOP ( 'NONE', ( #7244, #6551, #9686, #6560 ) ) ;
#2898 = VERTEX_POINT ( 'NONE', #7270 ) ;
#2899 = CARTESIAN_POINT ( 'NONE',  ( 114.6731053250840233, 0.000000000000000000, 139.1143251403882459 ) ) ;
#2900 = VECTOR ( 'NONE', #12536, 1000.000000000000000 ) ;
#2901 = ORIENTED_EDGE ( 'NONE', *, *, #9974, .F. ) ;
#2902 = DIRECTION ( 'NONE',  ( 0.000000000000000000, 1.734723475976817547E-15, -1.000000000000000000 ) ) ;
#2903 = CARTESIAN_POINT ( 'NONE',  ( 69.43435019845104250, -3.089082358326208588, 71.61404092738268901 ) ) ;
#2904 = ORIENTED_EDGE ( 'NONE', *, *, #2745, .F. ) ;
#2905 = CIRCLE ( 'NONE', #12002, 7.000000000000000000 ) ;
#2906 = CARTESIAN_POINT ( 'NONE',  ( 0.000000000000000000, 21.75070940071315562, 33.00000000000012790 ) ) ;
#2907 = CARTESIAN_POINT ( 'NONE',  ( 20.86173033120691045, -72.24929059928631148, 7.000000000000000000 ) ) ;
#2908 = ORIENTED_EDGE ( 'NONE', *, *, #15154, .F. ) ;
#2909 = CARTESIAN_POINT ( 'NONE',  ( 29.30348265399867103, -64.16417350152767085, -3.791131921649141034 ) ) ;
#2910 = ORIENTED_EDGE ( 'NONE', *, *, #6357, .F. ) ;
#2911 = B_SPLINE_CURVE_WITH_KNOTS ( 'NONE', 3,
 ( #239, #8544, #1542, #8399 ),
 .UNSPECIFIED., .F., .F.,
 ( 4, 4 ),
 ( 0.000000000000000000, 0.003645914952990591488 ),
 .UNSPECIFIED. ) ;
#2912 = CARTESIAN_POINT ( 'NONE',  ( 27.25620696618382865, -52.24929059928630437, 3.946667064627068733 ) ) ;
#2913 = DIRECTION ( 'NONE',  ( -1.000000000000000000, 0.000000000000000000, 0.000000000000000000 ) ) ;
#2914 = CARTESIAN_POINT ( 'NONE',  ( -3.190546569013415379, 0.8906624217387615339, -48.00000000000012079 ) ) ;
#2915 = ADVANCED_FACE ( 'NONE', ( #4741 ), #12560, .F. ) ;
#2916 = CARTESIAN_POINT ( 'NONE',  ( -2.016677571526633510E-15, 23.25070940071368497, 139.1143251403882459 ) ) ;
#2917 = ORIENTED_EDGE ( 'NONE', *, *, #13409, .F. ) ;
#2918 = CARTESIAN_POINT ( 'NONE',  ( 50.01091543003727224, 21.75070940071325865, -33.00000000000012790 ) ) ;
#2919 = CIRCLE ( 'NONE', #10797, 3.694885682588112896 ) ;
#2920 = EDGE_CURVE ( 'NONE', #8990, #10817, #14526, .T. ) ;
#2921 = ORIENTED_EDGE ( 'NONE', *, *, #11765, .F. ) ;
#2922 = VERTEX_POINT ( 'NONE', #1109 ) ;
#2923 = EDGE_CURVE ( 'NONE', #3601, #1918, #7158, .T. ) ;
#2924 = EDGE_CURVE ( 'NONE', #10383, #8896, #5822, .T. ) ;
#2925 = VERTEX_POINT ( 'NONE', #4660 ) ;
#2926 = FACE_OUTER_BOUND ( 'NONE', #7899, .T. ) ;
#2927 = DIRECTION ( 'NONE',  ( -0.4848096202550659650, -0.8746197071345572782, -0.000000000000000000 ) ) ;
#2928 = DIRECTION ( 'NONE',  ( 0.000000000000000000, -0.000000000000000000, 1.000000000000000000 ) ) ;
#2929 = AXIS2_PLACEMENT_3D ( 'NONE', #3710, #4720, #2484 ) ;
#2930 = EDGE_CURVE ( 'NONE', #7613, #1961, #11081, .T. ) ;
#2931 = CARTESIAN_POINT ( 'NONE',  ( -16.99999999999998579, 2.256146146571129218, 36.00000000000012079 ) ) ;
#2932 = ORIENTED_EDGE ( 'NONE', *, *, #2144, .T. ) ;
#2933 = LINE ( 'NONE', #7625, #11739 ) ;
#2934 = CARTESIAN_POINT ( 'NONE',  ( 64.71315123357256027, -11.54339494126895005, 71.67174403569786989 ) ) ;
#2935 = CARTESIAN_POINT ( 'NONE',  ( -10.97058782713534164, -9.028420861780718454, -48.26891069786831423 ) ) ;
#2936 = CARTESIAN_POINT ( 'NONE',  ( -9.268887740808379405, 2.359106894006888666, 47.70917337021941762 ) ) ;
#2937 = CARTESIAN_POINT ( 'NONE',  ( 10.00023835250150128, -61.42570632716525125, -2.132522520905388852 ) ) ;
#2938 = ORIENTED_EDGE ( 'NONE', *, *, #12012, .T. ) ;
#2939 = CARTESIAN_POINT ( 'NONE',  ( 54.00000000000000711, -2.249290599286311032, 33.00000000000012790 ) ) ;
#2940 = AXIS2_PLACEMENT_3D ( 'NONE', #11432, #7760, #11285 ) ;
#2941 = VECTOR ( 'NONE', #5173, 1000.000000000000000 ) ;
#2942 = ADVANCED_FACE ( 'NONE', ( #8574 ), #14429, .F. ) ;
#2943 = DIRECTION ( 'NONE',  ( -0.8746197071345571672, 0.4848096202550659650, 0.000000000000000000 ) ) ;
#2944 = VERTEX_POINT ( 'NONE', #13276 ) ;
#2945 =( LENGTH_UNIT ( ) NAMED_UNIT ( * ) SI_UNIT ( .MILLI., .METRE. ) );
#2946 = DIRECTION ( 'NONE',  ( -0.8420378618367723167, -0.5394184268574414576, -0.000000000000000000 ) ) ;
#2947 = B_SPLINE_CURVE_WITH_KNOTS ( 'NONE', 3,
 ( #9612, #8376, #14294, #14378, #8461, #13144, #2595, #2673 ),
 .UNSPECIFIED., .F., .F.,
 ( 4, 2, 2, 4 ),
 ( 5.291795217412410304E-17, 0.001077686929059509672, 0.002155373858118966434, 0.004310747716237871285 ),
 .UNSPECIFIED. ) ;
#2948 =( NAMED_UNIT ( * ) SI_UNIT ( $, .STERADIAN. ) SOLID_ANGLE_UNIT ( ) );
#2949 = CARTESIAN_POINT ( 'NONE',  ( 73.69809405469877106, 29.52935533987996664, -21.00807340887166674 ) ) ;
#2950 = ORIENTED_EDGE ( 'NONE', *, *, #11121, .F. ) ;
#2951 = ADVANCED_FACE ( 'NONE', ( #13565 ), #2867, .F. ) ;
#2952 = DIRECTION ( 'NONE',  ( 0.8208219420614786266, -0.4549890321264269955, -0.3453061251629919726 ) ) ;
#2953 = AXIS2_PLACEMENT_3D ( 'NONE', #2490, #2338, #9346 ) ;
#2954 = LINE ( 'NONE', #8714, #5680 ) ;
#2955 =( NAMED_UNIT ( * ) SI_UNIT ( $, .STERADIAN. ) SOLID_ANGLE_UNIT ( ) );
#2956 = CARTESIAN_POINT ( 'NONE',  ( -24.60804510916187837, -7.057608296800744085, -47.99579695943414492 ) ) ;
#2957 = EDGE_CURVE ( 'NONE', #12265, #3301, #14572, .T. ) ;
#2958 = EDGE_LOOP ( 'NONE', ( #7879, #14398, #10143, #14155, #8547, #1210, #8196, #2978, #2185 ) ) ;
#2959 = CARTESIAN_POINT ( 'NONE',  ( 34.39473169496078242, -50.37334675433798026, -2.732818608182232989 ) ) ;
#2960 = ORIENTED_EDGE ( 'NONE', *, *, #1567, .F. ) ;
#2961 = CARTESIAN_POINT ( 'NONE',  ( -25.21252699837112132, -6.998437922861946880, 48.50000000000012079 ) ) ;
#2962 = CARTESIAN_POINT ( 'NONE',  ( -16.99999999999998579, -2.249290599286303927, 48.00000000000012079 ) ) ;
#2963 = CIRCLE ( 'NONE', #4934, 0.9999999999999977796 ) ;
#2964 = ORIENTED_EDGE ( 'NONE', *, *, #7226, .F. ) ;
#2965 = CARTESIAN_POINT ( 'NONE',  ( 80.00000000000001421, -72.24929059928631148, -34.99999999999999289 ) ) ;
#2966 = DIRECTION ( 'NONE',  ( -0.000000000000000000, 0.000000000000000000, 1.000000000000000000 ) ) ;
#2967 = EDGE_CURVE ( 'NONE', #1905, #14376, #12036, .T. ) ;
#2968 = EDGE_CURVE ( 'NONE', #6172, #4927, #4433, .T. ) ;
#2969 = ORIENTED_EDGE ( 'NONE', *, *, #4653, .F. ) ;
#2970 = CARTESIAN_POINT ( 'NONE',  ( 61.57781019154727176, -5.828480965243416634, 62.84860122826521689 ) ) ;
#2971 = AXIS2_PLACEMENT_3D ( 'NONE', #7820, #4420, #12506 ) ;
#2972 = CARTESIAN_POINT ( 'NONE',  ( 12.02094163398139948, -52.24929059928630437, 4.175384597093459327 ) ) ;
#2973 = CARTESIAN_POINT ( 'NONE',  ( 105.5545870572953930, 23.25070940071369563, 13.14990448602692474 ) ) ;
#2974 = DIRECTION ( 'NONE',  ( 1.000000000000000000, 0.000000000000000000, 0.000000000000000000 ) ) ;
#2975 = VERTEX_POINT ( 'NONE', #12182 ) ;
#2976 = CARTESIAN_POINT ( 'NONE',  ( -16.99999999999998579, -2.249290599286303927, 38.00000000000012079 ) ) ;
#2977 = AXIS2_PLACEMENT_3D ( 'NONE', #14523, #8672, #11055 ) ;
#2978 = ORIENTED_EDGE ( 'NONE', *, *, #11176, .T. ) ;
#2979 = LINE ( 'NONE', #12367, #6410 ) ;
#2980 = VECTOR ( 'NONE', #14639, 1000.000000000000000 ) ;
#2981 = ORIENTED_EDGE ( 'NONE', *, *, #4998, .F. ) ;
#2982 = CYLINDRICAL_SURFACE ( 'NONE', #15001, 2.999999999999999112 ) ;
#2983 = ADVANCED_FACE ( 'NONE', ( #7646 ), #6403, .F. ) ;
#2984 = CIRCLE ( 'NONE', #6414, 0.5000000000000000000 ) ;
#2985 = EDGE_CURVE ( 'NONE', #4765, #3836, #11556, .T. ) ;
#2986 = CARTESIAN_POINT ( 'NONE',  ( 51.75774672102440377, 23.25070940071368852, 139.1143251403882459 ) ) ;
#2987 = ORIENTED_EDGE ( 'NONE', *, *, #5655, .T. ) ;
#2988 = CARTESIAN_POINT ( 'NONE',  ( 58.00000000000000711, -6.754727345143743733, 36.00000000000012079 ) ) ;
#2989 = DIRECTION ( 'NONE',  ( 0.000000000000000000, 0.000000000000000000, 1.000000000000000000 ) ) ;
#2990 = ORIENTED_EDGE ( 'NONE', *, *, #13123, .F. ) ;
#2991 = AXIS2_PLACEMENT_3D ( 'NONE', #10271, #4410, #5656 ) ;
#2992 = ORIENTED_EDGE ( 'NONE', *, *, #10935, .F. ) ;
#2993 = VECTOR ( 'NONE', #11770, 1000.000000000000000 ) ;
#2994 = AXIS2_PLACEMENT_3D ( 'NONE', #1991, #15008, #13699 ) ;
#2995 = CARTESIAN_POINT ( 'NONE',  ( 12.03298173962126327, -53.28399145779480506, -4.141535524925033407 ) ) ;
#2996 = LINE ( 'NONE', #5610, #10659 ) ;
#2997 = CARTESIAN_POINT ( 'NONE',  ( -1.197457146693678531, -2.220571218158920779, 48.50000000000012079 ) ) ;
#2998 = ORIENTED_EDGE ( 'NONE', *, *, #7311, .T. ) ;
#2999 = CARTESIAN_POINT ( 'NONE',  ( -6.999999999999987566, -2.249290599286157821, 33.00000000000012790 ) ) ;
#3000 = ORIENTED_EDGE ( 'NONE', *, *, #1099, .F. ) ;
#3001 = EDGE_LOOP ( 'NONE', ( #13316, #731, #1779, #1003 ) ) ;
#3002 = AXIS2_PLACEMENT_3D ( 'NONE', #14403, #13102, #10865 ) ;
#3003 = VERTEX_POINT ( 'NONE', #14637 ) ;
#3004 = VECTOR ( 'NONE', #2493, 1000.000000000000000 ) ;
#3005 = DIRECTION ( 'NONE',  ( 0.000000000000000000, -0.000000000000000000, 1.000000000000000000 ) ) ;
#3006 = AXIS2_PLACEMENT_3D ( 'NONE', #14105, #7100, #11786 ) ;
#3007 = CARTESIAN_POINT ( 'NONE',  ( 20.86173033120691045, -52.24929059928630437, 3.000000000000000888 ) ) ;
#3008 = ADVANCED_FACE ( 'NONE', ( #4019 ), #7425, .F. ) ;
#3009 = CARTESIAN_POINT ( 'NONE',  ( -2.688903428702175252E-15, 23.25070940071368142, 139.1143251403882459 ) ) ;
#3010 = CARTESIAN_POINT ( 'NONE',  ( -12.14523415828296216, -9.827631355817223024, -48.50000000000012079 ) ) ;
#3011 = VERTEX_POINT ( 'NONE', #8791 ) ;
#3012 = CARTESIAN_POINT ( 'NONE',  ( 64.97177248905298086, -11.36467339961058443, 72.35795077993141433 ) ) ;
#3013 = AXIS2_PLACEMENT_3D ( 'NONE', #2590, #12991, #11671 ) ;
#3014 = DIRECTION ( 'NONE',  ( -1.000000000000000000, -1.734723475976807292E-15, 0.000000000000000000 ) ) ;
#3015 = CARTESIAN_POINT ( 'NONE',  ( 40.33162949095117966, 21.75070940071319114, 33.00000000000012790 ) ) ;
#3016 = DIRECTION ( 'NONE',  ( 0.000000000000000000, -1.000000000000000000, 0.000000000000000000 ) ) ;
#3017 = VECTOR ( 'NONE', #6861, 1000.000000000000000 ) ;
#3018 = ORIENTED_EDGE ( 'NONE', *, *, #2923, .F. ) ;
#3019 = CARTESIAN_POINT ( 'NONE',  ( 33.63076355350840174, -56.34136508318270842, 1.853100783822632325 ) ) ;
#3020 = ADVANCED_FACE ( 'NONE', ( #5114 ), #11033, .F. ) ;
#3021 = AXIS2_PLACEMENT_3D ( 'NONE', #3933, #7180, #1404 ) ;
#3022 = EDGE_CURVE ( 'NONE', #7867, #1978, #2954, .T. ) ;
#3023 = CARTESIAN_POINT ( 'NONE',  ( -8.787473001628836045, 2.499856724289236887, 48.50000000000012079 ) ) ;
#3024 = ORIENTED_EDGE ( 'NONE', *, *, #8643, .T. ) ;
#3025 = FACE_OUTER_BOUND ( 'NONE', #3144, .T. ) ;
#3026 = CARTESIAN_POINT ( 'NONE',  ( 80.18290120114222930, 25.52935533987996664, 21.00807340887166674 ) ) ;
#3027 = VERTEX_POINT ( 'NONE', #1576 ) ;
#3028 = CARTESIAN_POINT ( 'NONE',  ( 11.79087746573607909, -53.28557432868839072, 4.055360768046006648 ) ) ;
#3029 = AXIS2_PLACEMENT_3D ( 'NONE', #7140, #7066, #11599 ) ;
#3030 = EDGE_CURVE ( 'NONE', #9111, #6074, #9623, .T. ) ;
#3031 = EDGE_CURVE ( 'NONE', #3027, #4458, #13994, .T. ) ;
#3032 = DIRECTION ( 'NONE',  ( 0.000000000000000000, 0.000000000000000000, -1.000000000000000000 ) ) ;
#3033 = FACE_OUTER_BOUND ( 'NONE', #4631, .T. ) ;
#3034 =( BOUNDED_SURFACE ( )  B_SPLINE_SURFACE ( 3, 2, ( 
 ( #11855, #14172, #14326 ),
 ( #1390, #385, #6023 ),
 ( #164, #3774, #5081 ),
 ( #244, #9787, #3920 ),
 ( #8615, #13313, #13250 ),
 ( #9564, #3625, #3698 ),
 ( #9718, #14399, #8403 ),
 ( #8482, #3841, #7473 ) ),
 .UNSPECIFIED., .F., .F., .F. ) 
 B_SPLINE_SURFACE_WITH_KNOTS ( ( 4, 2, 2, 4 ),
 ( 3, 3 ),
 ( 0.000000000000000000, 0.001129222206655581574, 0.002258444413311163149, 0.004516888826622326297 ),
 ( 0.000000000000000000, 1.000000000000000000 ),
 .UNSPECIFIED. ) 
 GEOMETRIC_REPRESENTATION_ITEM ( )  RATIONAL_B_SPLINE_SURFACE ( (
 ( 1.000000000000000000, 0.7071067811864936159, 1.000000000000000000),
 ( 1.000000000000000000, 0.7608707698420138499, 1.000000000000000000),
 ( 1.000000000000000000, 0.8047257278452277784, 1.000000000000000000),
 ( 1.000000000000000000, 0.8783509392183566078, 1.000000000000000000),
 ( 1.000000000000000000, 0.9081758943102266057, 1.000000000000000000),
 ( 1.000000000000000000, 0.9781389570711758186, 1.000000000000000000),
 ( 1.000000000000000000, 0.9996704379314563793, 1.000000000000000000),
 ( 1.000000000000000000, 1.000000000000000000, 1.000000000000000000) ) ) 
 REPRESENTATION_ITEM ( '' )  SURFACE ( )  );
#3035 = CARTESIAN_POINT ( 'NONE',  ( 27.95143033160315582, -67.83931925369921601, -3.638954064322521553 ) ) ;
#3036 = VERTEX_POINT ( 'NONE', #5265 ) ;
#3037 = AXIS2_PLACEMENT_3D ( 'NONE', #4264, #11343, #6733 ) ;
#3038 = DIRECTION ( 'NONE',  ( 0.000000000000000000, 0.000000000000000000, 1.000000000000000000 ) ) ;
#3039 = VECTOR ( 'NONE', #6310, 1000.000000000000000 ) ;
#3040 = VERTEX_POINT ( 'NONE', #12340 ) ;
#3041 = CARTESIAN_POINT ( 'NONE',  ( 29.35555050496136786, -52.24929059928630437, -3.199931146564429341 ) ) ;
#3042 = CARTESIAN_POINT ( 'NONE',  ( 80.00000000000001421, -85.24929059928629727, 8.000000000000001776 ) ) ;
#3043 = ORIENTED_EDGE ( 'NONE', *, *, #11823, .F. ) ;
#3044 = CARTESIAN_POINT ( 'NONE',  ( 60.40269930420516431, 2.204737408716291647, 62.84860122826521689 ) ) ;
#3045 = CARTESIAN_POINT ( 'NONE',  ( 13.87384783255121690, -69.39711819508849544, -3.799217554615847980 ) ) ;
#3046 = CARTESIAN_POINT ( 'NONE',  ( 12.66974950169162284, -64.60713873539378937, 3.212402267261584399 ) ) ;
#3047 = DIRECTION ( 'NONE',  ( 2.102695122396130163E-16, -1.682156097916904130E-15, 1.000000000000000000 ) ) ;
#3048 = CARTESIAN_POINT ( 'NONE',  ( 108.0866310645538562, 21.75070940071366365, -13.14990448602693007 ) ) ;
#3049 = CARTESIAN_POINT ( 'NONE',  ( 0.5043391135745837195, 0.8906624217387615339, -48.50000000000012079 ) ) ;
#3050 = ADVANCED_FACE ( 'NONE', ( #1795 ), #6488, .T. ) ;
#3051 = DIRECTION ( 'NONE',  ( 0.000000000000000000, 0.000000000000000000, 1.000000000000000000 ) ) ;
#3052 = ORIENTED_EDGE ( 'NONE', *, *, #5683, .F. ) ;
#3053 = CARTESIAN_POINT ( 'NONE',  ( 9.200644618036292854, -59.06479067038041819, 2.757123406423321210 ) ) ;
#3054 = EDGE_CURVE ( 'NONE', #4027, #143, #12657, .T. ) ;
#3055 = ORIENTED_EDGE ( 'NONE', *, *, #9895, .T. ) ;
#3056 = CARTESIAN_POINT ( 'NONE',  ( 32.73440452410881107, -55.35059346084329235, -2.955710789589959919 ) ) ;
#3057 = ORIENTED_EDGE ( 'NONE', *, *, #7991, .T. ) ;
#3058 = CARTESIAN_POINT ( 'NONE',  ( 27.94158133900394958, -67.90279320103996952, 3.641642753168639501 ) ) ;
#3059 = CARTESIAN_POINT ( 'NONE',  ( 52.35373241494735197, -0.8423457118892125894, 60.61639468829817190 ) ) ;
#3060 = CARTESIAN_POINT ( 'NONE',  ( 58.00000000000000711, -2.249290599286311032, 38.00000000000012079 ) ) ;
#3061 = CARTESIAN_POINT ( 'NONE',  ( -12.00298721683875236, -9.736506449376861383, 48.44214661497220931 ) ) ;
#3062 = VERTEX_POINT ( 'NONE', #10422 ) ;
#3063 = FACE_OUTER_BOUND ( 'NONE', #13077, .T. ) ;
#3064 = ORIENTED_EDGE ( 'NONE', *, *, #10647, .F. ) ;
#3065 = CARTESIAN_POINT ( 'NONE',  ( -25.21252699837112132, -6.998437922861946880, -48.50000000000012079 ) ) ;
#3066 = DIRECTION ( 'NONE',  ( -1.000000000000000000, -0.000000000000000000, -0.000000000000000000 ) ) ;
#3067 = DIRECTION ( 'NONE',  ( -0.000000000000000000, 1.000000000000000000, -0.000000000000000000 ) ) ;
#3068 = EDGE_CURVE ( 'NONE', #3756, #446, #14953, .T. ) ;
#3069 = ADVANCED_FACE ( 'NONE', ( #9190 ), #15111, .F. ) ;
#3070 = CARTESIAN_POINT ( 'NONE',  ( 58.80593636315131079, 3.245402227105440129, 48.51982618741349285 ) ) ;
#3071 = EDGE_LOOP ( 'NONE', ( #13368, #4254, #3209, #14024, #371 ) ) ;
#3072 = CARTESIAN_POINT ( 'NONE',  ( -16.99999999999998579, -2.249290599286303927, 38.00000000000012079 ) ) ;
#3073 = ORIENTED_EDGE ( 'NONE', *, *, #10860, .T. ) ;
#3074 = ORIENTED_EDGE ( 'NONE', *, *, #7357, .T. ) ;
#3075 = ORIENTED_EDGE ( 'NONE', *, *, #13143, .F. ) ;
#3076 = CARTESIAN_POINT ( 'NONE',  ( 72.26742264675378635, -14.73126838498887281, 75.19766410831374515 ) ) ;
#3077 = CARTESIAN_POINT ( 'NONE',  ( 0.000000000000000000, 21.75070940071366365, -33.00000000000012790 ) ) ;
#3078 = CARTESIAN_POINT ( 'NONE',  ( 35.49198652140812982, 0.000000000000000000, -33.00000000000012790 ) ) ;
#3079 = ORIENTED_EDGE ( 'NONE', *, *, #6532, .T. ) ;
#3080 = ADVANCED_FACE ( 'NONE', ( #13639 ), #8950, .F. ) ;
#3081 = CARTESIAN_POINT ( 'NONE',  ( 48.84742675818896629, 2.824063592853377269, 61.61639468829817190 ) ) ;
#3082 = CARTESIAN_POINT ( 'NONE',  ( 69.45530162631038706, -2.717604841179691366, 76.41417248176652777 ) ) ;
#3083 = CARTESIAN_POINT ( 'NONE',  ( 18.24487436548682950, -53.24929059928630437, -6.492462156583989064 ) ) ;
#3084 = CARTESIAN_POINT ( 'NONE',  ( 11.98773490706720324, -63.50313342087172686, -3.632148419031555608 ) ) ;
#3085 = ORIENTED_EDGE ( 'NONE', *, *, #5702, .T. ) ;
#3086 = CARTESIAN_POINT ( 'NONE',  ( 69.98312355368540238, -3.182969857497201183, 73.06092304798380610 ) ) ;
#3087 = CARTESIAN_POINT ( 'NONE',  ( 88.00000000000001421, 10.75070940071369208, 33.00000000000012790 ) ) ;
#3088 = EDGE_LOOP ( 'NONE', ( #15197, #7111, #13663, #4211 ) ) ;
#3089 = CARTESIAN_POINT ( 'NONE',  ( 13.86173033120691223, -69.39711819508849544, -3.619682905202625811 ) ) ;
#3090 = TOROIDAL_SURFACE ( 'NONE', #6523, 3.694885682587998765, 0.5000000000000000000 ) ;
#3091 = DIRECTION ( 'NONE',  ( -0.000000000000000000, 0.000000000000000000, 1.000000000000000000 ) ) ;
#3092 = CARTESIAN_POINT ( 'NONE',  ( 47.27423575335444639, 23.25070940071368852, 33.00000000000012790 ) ) ;
#3093 = ORIENTED_EDGE ( 'NONE', *, *, #12852, .F. ) ;
#3094 = CARTESIAN_POINT ( 'NONE',  ( 10.21747785520277851, -53.84004999663768132, 3.478067438360142205 ) ) ;
#3095 = CARTESIAN_POINT ( 'NONE',  ( 80.00000000000001421, -76.24929059928631148, 6.000000000000000000 ) ) ;
#3096 = CARTESIAN_POINT ( 'NONE',  ( 53.41380296247595538, -0.1096349785133995947, 48.51982618741349285 ) ) ;
#3097 = DIRECTION ( 'NONE',  ( -0.000000000000000000, 1.000000000000000000, -0.000000000000000000 ) ) ;
#3098 = VECTOR ( 'NONE', #3632, 1000.000000000000000 ) ;
#3099 = VERTEX_POINT ( 'NONE', #13875 ) ;
#3100 = DIRECTION ( 'NONE',  ( 1.000000000000000000, 0.000000000000000000, 0.000000000000000000 ) ) ;
#3101 = ORIENTED_EDGE ( 'NONE', *, *, #8041, .F. ) ;
#3102 = EDGE_CURVE ( 'NONE', #13132, #4131, #10107, .T. ) ;
#3103 = CARTESIAN_POINT ( 'NONE',  ( 25.53134746123848231, -53.25924031079294707, -5.665074923594188405 ) ) ;
#3104 = LINE ( 'NONE', #4329, #14070 ) ;
#3105 = EDGE_CURVE ( 'NONE', #1762, #3899, #5647, .T. ) ;
#3106 = EDGE_CURVE ( 'NONE', #1863, #1580, #7956, .T. ) ;
#3107 = ORIENTED_EDGE ( 'NONE', *, *, #4323, .T. ) ;
#3108 = CARTESIAN_POINT ( 'NONE',  ( 62.67308791069655882, 29.52935533987996664, 33.00000000000014211 ) ) ;
#3109 = CARTESIAN_POINT ( 'NONE',  ( 20.86173033120691045, -53.24929059928630437, 0.000000000000000000 ) ) ;
#3110 = VERTEX_POINT ( 'NONE', #3095 ) ;
#3111 = AXIS2_PLACEMENT_3D ( 'NONE', #10141, #9059, #14828 ) ;
#3112 = CIRCLE ( 'NONE', #10985, 0.5000000000000000000 ) ;
#3113 = CARTESIAN_POINT ( 'NONE',  ( 13.39143123690971571, -66.31583591551516577, 4.137138225902095456 ) ) ;
#3114 = SHAPE_REPRESENTATION ( 'Slot', ( #6315 ), #11962 ) ;
#3115 = EDGE_CURVE ( 'NONE', #8264, #1089, #6071, .T. ) ;
#3116 = CARTESIAN_POINT ( 'NONE',  ( 10.22665806587732362, -53.84195147944168269, 3.481029309661981319 ) ) ;
#3117 = CARTESIAN_POINT ( 'NONE',  ( 29.99044527668438320, -52.28496698959959588, -3.026492948547165440 ) ) ;
#3118 = VECTOR ( 'NONE', #7275, 1000.000000000000000 ) ;
#3119 = DIRECTION ( 'NONE',  ( 0.000000000000000000, 0.000000000000000000, 1.000000000000000000 ) ) ;
#3120 = CARTESIAN_POINT ( 'NONE',  ( -24.65452791727695114, 3.133494033999976391, -48.02161282446748203 ) ) ;
#3121 = ORIENTED_EDGE ( 'NONE', *, *, #3711, .F. ) ;
#3122 = CIRCLE ( 'NONE', #11731, 0.7892041907098253928 ) ;
#3123 = LINE ( 'NONE', #12142, #1401 ) ;
#3124 = ORIENTED_EDGE ( 'NONE', *, *, #3628, .F. ) ;
#3125 = FACE_OUTER_BOUND ( 'NONE', #601, .T. ) ;
#3126 = EDGE_LOOP ( 'NONE', ( #3043, #2097, #8837, #5912 ) ) ;
#3127 = DIRECTION ( 'NONE',  ( 0.000000000000000000, 0.000000000000000000, 1.000000000000000000 ) ) ;
#3128 = CARTESIAN_POINT ( 'NONE',  ( 69.36208556723036622, -3.784586871655906570, 71.26433199163157894 ) ) ;
#3129 = CIRCLE ( 'NONE', #9545, 31.00000000000000000 ) ;
#3130 = CARTESIAN_POINT ( 'NONE',  ( -8.842479278987921631, -7.118053859731281463, -47.50000000000012079 ) ) ;
#3131 = CARTESIAN_POINT ( 'NONE',  ( 37.23881781239525424, 0.000000000000000000, 33.00000000000012790 ) ) ;
#3132 = VERTEX_POINT ( 'NONE', #5412 ) ;
#3133 = VECTOR ( 'NONE', #5474, 1000.000000000000000 ) ;
#3134 = ADVANCED_FACE ( 'NONE', ( #6634 ), #11319, .T. ) ;
#3135 = CARTESIAN_POINT ( 'NONE',  ( -65.00000000000001421, -85.27429059928630295, 19.99999999999999645 ) ) ;
#3136 = AXIS2_PLACEMENT_3D ( 'NONE', #1243, #8182, #22 ) ;
#3137 = ORIENTED_EDGE ( 'NONE', *, *, #12288, .F. ) ;
#3138 = CYLINDRICAL_SURFACE ( 'NONE', #13502, 4.000000000000003553 ) ;
#3139 = CARTESIAN_POINT ( 'NONE',  ( 9.328516978903417467, -53.50439862579597161, -3.186601206343369075 ) ) ;
#3140 = DIRECTION ( 'NONE',  ( 1.000000000000000000, 0.000000000000000000, 0.000000000000000000 ) ) ;
#3141 = CARTESIAN_POINT ( 'NONE',  ( -10.99067925302910176, -8.982598353005794678, 48.14374739243442747 ) ) ;
#3142 = ORIENTED_EDGE ( 'NONE', *, *, #13697, .T. ) ;
#3143 = AXIS2_PLACEMENT_3D ( 'NONE', #10152, #6834, #10305 ) ;
#3144 = EDGE_LOOP ( 'NONE', ( #11058, #5212, #9723, #10671 ) ) ;
#3145 = PLANE ( 'NONE',  #12481 ) ;
#3146 = ORIENTED_EDGE ( 'NONE', *, *, #6594, .F. ) ;
#3147 = DIRECTION ( 'NONE',  ( 1.000000000000000000, 0.000000000000000000, 0.000000000000000000 ) ) ;
#3148 = VECTOR ( 'NONE', #15223, 1000.000000000000000 ) ;
#3149 = ORIENTED_EDGE ( 'NONE', *, *, #5378, .T. ) ;
#3150 = ORIENTED_EDGE ( 'NONE', *, *, #13449, .T. ) ;
#3151 = CARTESIAN_POINT ( 'NONE',  ( 9.755347871979424212, -60.26979819505855573, -2.885043711493008090 ) ) ;
#3152 = CARTESIAN_POINT ( 'NONE',  ( -23.00932074697458773, 4.484017154434125629, -48.14374739243680068 ) ) ;
#3153 = EDGE_CURVE ( 'NONE', #8990, #4595, #3176, .T. ) ;
#3154 = EDGE_CURVE ( 'NONE', #8543, #12651, #5323, .T. ) ;
#3155 = LINE ( 'NONE', #11300, #5068 ) ;
#3156 = SURFACE_STYLE_USAGE ( .BOTH. , #13929 ) ;
#3157 = ORIENTED_EDGE ( 'NONE', *, *, #11189, .F. ) ;
#3158 = PLANE ( 'NONE',  #8151 ) ;
#3159 = DIRECTION ( 'NONE',  ( 0.4848096202550659650, 0.8746197071345572782, 0.000000000000000000 ) ) ;
#3160 = CARTESIAN_POINT ( 'NONE',  ( 58.00000000000000711, -2.249290599286311032, 33.00000000000012790 ) ) ;
#3161 = CARTESIAN_POINT ( 'NONE',  ( 80.00000000000001421, -72.24929059928631148, 34.99999999999999289 ) ) ;
#3162 = ORIENTED_EDGE ( 'NONE', *, *, #2568, .T. ) ;
#3163 = DIRECTION ( 'NONE',  ( 0.000000000000000000, 0.000000000000000000, 1.000000000000000000 ) ) ;
#3164 = FACE_OUTER_BOUND ( 'NONE', #7169, .T. ) ;
#3165 = VERTEX_POINT ( 'NONE', #1093 ) ;
#3166 = CARTESIAN_POINT ( 'NONE',  ( -30.80945343098651890, -5.389243620311580329, -58.00000000000012079 ) ) ;
#3167 = CARTESIAN_POINT ( 'NONE',  ( 43.00000000000000711, 10.25070940071368497, 33.00000000000012790 ) ) ;
#3168 = ADVANCED_FACE ( 'NONE', ( #9338 ), #11642, .T. ) ;
#3169 = ADVANCED_FACE ( 'NONE', ( #179 ), #4874, .T. ) ;
#3170 = DIRECTION ( 'NONE',  ( -0.000000000000000000, -0.000000000000000000, 1.000000000000000000 ) ) ;
#3171 = CARTESIAN_POINT ( 'NONE',  ( 27.33382790127957662, -69.39711819508849544, -4.502057496415715399 ) ) ;
#3172 = VERTEX_POINT ( 'NONE', #10649 ) ;
#3173 = CARTESIAN_POINT ( 'NONE',  ( 80.00000000000001421, -74.24929059928631148, 32.00000000000000000 ) ) ;
#3174 = FACE_OUTER_BOUND ( 'NONE', #12005, .T. ) ;
#3175 = CARTESIAN_POINT ( 'NONE',  ( -16.99999999999998579, -2.249290599286303927, -48.00000000000012079 ) ) ;
#3176 = CIRCLE ( 'NONE', #8816, 9.500000000000001776 ) ;
#3177 = VECTOR ( 'NONE', #12177, 1000.000000000000000 ) ;
#3178 = PLANE ( 'NONE',  #12328 ) ;
#3179 = ORIENTED_EDGE ( 'NONE', *, *, #9295, .F. ) ;
#3180 = FACE_OUTER_BOUND ( 'NONE', #7828, .T. ) ;
#3181 = VERTEX_POINT ( 'NONE', #11714 ) ;
#3182 = CARTESIAN_POINT ( 'NONE',  ( 20.86173033120691045, -57.24929059928630437, 0.000000000000000000 ) ) ;
#3183 = CARTESIAN_POINT ( 'NONE',  ( -21.16581936427349575, -2.249290599286304371, -50.00000000000012079 ) ) ;
#3184 = ORIENTED_EDGE ( 'NONE', *, *, #7284, .F. ) ;
#3185 = CYLINDRICAL_SURFACE ( 'NONE', #1786, 0.7892041907098262810 ) ;
#3186 = DIRECTION ( 'NONE',  ( 0.000000000000000000, 0.000000000000000000, 1.000000000000000000 ) ) ;
#3187 = VECTOR ( 'NONE', #7429, 1000.000000000000000 ) ;
#3188 = CARTESIAN_POINT ( 'NONE',  ( 9.826704175994500190, -61.28862151863886965, -2.085432713781506742 ) ) ;
#3189 = EDGE_CURVE ( 'NONE', #14936, #3904, #9655, .T. ) ;
#3190 = CARTESIAN_POINT ( 'NONE',  ( 120.9867508182053086, -31.44664636084115017, 54.40673322733725570 ) ) ;
#3191 = CARTESIAN_POINT ( 'NONE',  ( 32.23489539772602797, -59.84608319322163794, 2.809346289343019443 ) ) ;
#3192 = CARTESIAN_POINT ( 'NONE',  ( 118.0000000000000568, 2.046973701652633381E-13, -33.00000000000012790 ) ) ;
#3193 = EDGE_CURVE ( 'NONE', #3752, #11723, #5389, .T. ) ;
#3194 = EDGE_CURVE ( 'NONE', #5487, #2975, #110, .T. ) ;
#3195 = LINE ( 'NONE', #2973, #12889 ) ;
#3196 = LINE ( 'NONE', #7895, #9280 ) ;
#3197 = AXIS2_PLACEMENT_3D ( 'NONE', #11203, #13594, #5213 ) ;
#3198 = ORIENTED_EDGE ( 'NONE', *, *, #14960, .T. ) ;
#3199 = CARTESIAN_POINT ( 'NONE',  ( 13.46836618102747885, -61.89662211388733937, -4.174060188899890278 ) ) ;
#3200 = ORIENTED_EDGE ( 'NONE', *, *, #12234, .F. ) ;
#3201 = EDGE_CURVE ( 'NONE', #2664, #7882, #12514, .T. ) ;
#3202 = CARTESIAN_POINT ( 'NONE',  ( 32.52281604437752804, -59.06479067038042530, -2.757123406422443690 ) ) ;
#3203 = ORIENTED_EDGE ( 'NONE', *, *, #13971, .F. ) ;
#3204 = CARTESIAN_POINT ( 'NONE',  ( -65.00000000000001421, -85.27429059928630295, 22.50000000000000000 ) ) ;
#3205 = DIRECTION ( 'NONE',  ( -0.000000000000000000, -0.000000000000000000, -1.000000000000000000 ) ) ;
#3206 = DIRECTION ( 'NONE',  ( 1.000000000000000000, 0.000000000000000000, 0.000000000000000000 ) ) ;
#3207 = FACE_OUTER_BOUND ( 'NONE', #4528, .T. ) ;
#3208 = DIRECTION ( 'NONE',  ( -0.000000000000000000, -0.000000000000000000, 1.000000000000000000 ) ) ;
#3209 = ORIENTED_EDGE ( 'NONE', *, *, #6230, .T. ) ;
#3210 = EDGE_CURVE ( 'NONE', #7396, #1788, #8190, .T. ) ;
#3211 = ADVANCED_FACE ( 'NONE', ( #9420 ), #14188, .T. ) ;
#3212 = DIRECTION ( 'NONE',  ( 0.000000000000000000, 0.000000000000000000, -1.000000000000000000 ) ) ;
#3213 = CARTESIAN_POINT ( 'NONE',  ( 8.965898960377726823, -53.92993659400900697, -2.218374547571393851 ) ) ;
#3214 = DIRECTION ( 'NONE',  ( 1.000000000000000000, 0.000000000000000000, 0.000000000000000000 ) ) ;
#3215 = AXIS2_PLACEMENT_3D ( 'NONE', #6235, #10923, #372 ) ;
#3216 = CARTESIAN_POINT ( 'NONE',  ( -10.31821280924931372, -8.288623256088383684, 47.74919337097148286 ) ) ;
#3217 = VERTEX_POINT ( 'NONE', #2333 ) ;
#3218 = CIRCLE ( 'NONE', #8625, 0.9999999999999993339 ) ;
#3219 = CARTESIAN_POINT ( 'NONE',  ( 32.90197589884652274, -57.33450387999030795, 2.749014434309863919 ) ) ;
#3220 = APPLICATION_CONTEXT ( 'automotive_design' ) ;
#3221 = ORIENTED_EDGE ( 'NONE', *, *, #12327, .F. ) ;
#3222 = CARTESIAN_POINT ( 'NONE',  ( -25.15752072101212278, 2.619472661158555038, 47.50000000000012079 ) ) ;
#3223 = ORIENTED_EDGE ( 'NONE', *, *, #6729, .F. ) ;
#3224 = AXIS2_PLACEMENT_3D ( 'NONE', #10041, #1866, #11406 ) ;
#3225 = FACE_OUTER_BOUND ( 'NONE', #5552, .T. ) ;
#3226 = PLANE ( 'NONE',  #2278 ) ;
#3227 = AXIS2_PLACEMENT_3D ( 'NONE', #4760, #9745, #4598 ) ;
#3228 = CARTESIAN_POINT ( 'NONE',  ( 9.347558955408640458, -54.69585338401583385, -3.125080077088496111 ) ) ;
#3229 = LINE ( 'NONE', #914, #11845 ) ;
#3230 = ORIENTED_EDGE ( 'NONE', *, *, #2793, .F. ) ;
#3231 = DIRECTION ( 'NONE',  ( 0.000000000000000000, -0.000000000000000000, 1.000000000000000000 ) ) ;
#3232 = CARTESIAN_POINT ( 'NONE',  ( 64.11356537587559501, -11.94785244090458853, 73.19766410831374515 ) ) ;
#3233 = DIRECTION ( 'NONE',  ( 0.000000000000000000, -0.000000000000000000, -1.000000000000000000 ) ) ;
#3234 = CARTESIAN_POINT ( 'NONE',  ( 10.62011700622559829, -60.64100864355887666, 2.132522520905388852 ) ) ;
#3235 = PLANE ( 'NONE',  #15227 ) ;
#3236 = ORIENTED_EDGE ( 'NONE', *, *, #1913, .T. ) ;
#3237 = AXIS2_PLACEMENT_3D ( 'NONE', #9408, #10327, #15021 ) ;
#3238 = CARTESIAN_POINT ( 'NONE',  ( 12.36791015745246014, -53.24929059928630437, -3.199931146564422679 ) ) ;
#3239 = AXIS2_PLACEMENT_3D ( 'NONE', #13771, #7932, #15159 ) ;
#3240 = ADVANCED_FACE ( 'NONE', ( #2567 ), #10799, .F. ) ;
#3241 = AXIS2_PLACEMENT_3D ( 'NONE', #13853, #14636, #5624 ) ;
#3242 = DIRECTION ( 'NONE',  ( 1.000000000000000000, 0.000000000000000000, 0.000000000000000000 ) ) ;
#3243 = VERTEX_POINT ( 'NONE', #3644 ) ;
#3244 = CARTESIAN_POINT ( 'NONE',  ( 27.33382790127957662, -69.39711819508849544, -4.502057496415715399 ) ) ;
#3245 = DIRECTION ( 'NONE',  ( 1.000000000000000000, 0.000000000000000000, 0.000000000000000000 ) ) ;
#3246 = VERTEX_POINT ( 'NONE', #7178 ) ;
#3247 = DIRECTION ( 'NONE',  ( 0.8746197071345571672, -0.4848096202550660205, 0.000000000000000000 ) ) ;
#3248 = DIRECTION ( 'NONE',  ( 0.000000000000000000, 0.000000000000000000, 1.000000000000000000 ) ) ;
#3249 = VERTEX_POINT ( 'NONE', #8268 ) ;
#3250 = CARTESIAN_POINT ( 'NONE',  ( -2.016677571526633510E-15, 23.25070940071368497, 139.1143251403882459 ) ) ;
#3251 = AXIS2_PLACEMENT_3D ( 'NONE', #3958, #4028, #11119 ) ;
#3252 = CIRCLE ( 'NONE', #7431, 1.000000000000000888 ) ;
#3253 = VECTOR ( 'NONE', #4554, 1000.000000000000000 ) ;
#3254 = CARTESIAN_POINT ( 'NONE',  ( -3.190546569013415379, 0.8906624217387615339, 48.00000000000012079 ) ) ;
#3255 = DIRECTION ( 'NONE',  ( -1.000000000000000000, 0.000000000000000000, 0.000000000000000000 ) ) ;
#3256 = AXIS2_PLACEMENT_3D ( 'NONE', #233, #13011, #11916 ) ;
#3257 = LINE ( 'NONE', #1094, #238 ) ;
#3258 = DIRECTION ( 'NONE',  ( -1.000000000000000000, 0.000000000000000000, 0.000000000000000000 ) ) ;
#3259 = ADVANCED_FACE ( 'NONE', ( #12958 ), #11871, .T. ) ;
#3260 = ORIENTED_EDGE ( 'NONE', *, *, #14534, .T. ) ;
#3261 = PRODUCT_DEFINITION ( 'UNKNOWN', '', #14928, #10440 ) ;
#3262 = VERTEX_POINT ( 'NONE', #12808 ) ;
#3263 = DIRECTION ( 'NONE',  ( -0.000000000000000000, -1.000000000000000000, -0.000000000000000000 ) ) ;
#3264 = AXIS2_PLACEMENT_3D ( 'NONE', #6802, #13886, #3340 ) ;
#3265 = EDGE_LOOP ( 'NONE', ( #7746, #11331, #9067, #13249 ) ) ;
#3266 = LINE ( 'NONE', #10114, #10605 ) ;
#3267 = CARTESIAN_POINT ( 'NONE',  ( 9.169527510129993786, -53.67350875049211112, 2.284939533141856494 ) ) ;
#3268 = VECTOR ( 'NONE', #14516, 1000.000000000000000 ) ;
#3269 = VERTEX_POINT ( 'NONE', #2252 ) ;
#3270 = DIRECTION ( 'NONE',  ( -1.000000000000000000, 0.000000000000000000, 0.000000000000000000 ) ) ;
#3271 = DIRECTION ( 'NONE',  ( -0.000000000000000000, 0.000000000000000000, -1.000000000000000000 ) ) ;
#3272 = AXIS2_PLACEMENT_3D ( 'NONE', #614, #8852, #9874 ) ;
#3273 = FACE_OUTER_BOUND ( 'NONE', #9368, .T. ) ;
#3274 = CARTESIAN_POINT ( 'NONE',  ( 32.23803895999753166, -53.36286701831910761, -2.383094873945970971 ) ) ;
#3275 = DIRECTION ( 'NONE',  ( -1.734723475976807094E-15, 1.000000000000000000, 0.000000000000000000 ) ) ;
#3276 = VECTOR ( 'NONE', #10833, 1000.000000000000000 ) ;
#3277 = CARTESIAN_POINT ( 'NONE',  ( 59.12196317473677709, -7.688259372168277928, 48.51982618741349285 ) ) ;
#3278 = CARTESIAN_POINT ( 'NONE',  ( 0.000000000000000000, 15.25070940071368497, 33.00000000000012790 ) ) ;
#3279 = CIRCLE ( 'NONE', #2555, 0.7892041907098262810 ) ;
#3280 = ORIENTED_EDGE ( 'NONE', *, *, #9258, .T. ) ;
#3281 = CARTESIAN_POINT ( 'NONE',  ( 12.72586251681365965, -51.89519585600351803, -4.215672594460507128 ) ) ;
#3282 = EDGE_LOOP ( 'NONE', ( #4650, #5105, #9693, #11992, #8256, #1503, #1203 ) ) ;
#3283 = CARTESIAN_POINT ( 'NONE',  ( 62.00000000000001421, -2.249290599286310588, -33.00000000000012790 ) ) ;
#3284 = ORIENTED_EDGE ( 'NONE', *, *, #5084, .F. ) ;
#3285 = DIRECTION ( 'NONE',  ( 0.000000000000000000, 0.000000000000000000, -1.000000000000000000 ) ) ;
#3286 = DIRECTION ( 'NONE',  ( -0.000000000000000000, -0.000000000000000000, -1.000000000000000000 ) ) ;
#3287 = DIRECTION ( 'NONE',  ( 0.5125013958363124900, 0.8586863916854809986, 0.000000000000000000 ) ) ;
#3288 = DIRECTION ( 'NONE',  ( 1.000000000000000000, 0.000000000000000000, 0.000000000000000000 ) ) ;
#3289 = CIRCLE ( 'NONE', #9903, 0.5000000000000004441 ) ;
#3290 = DIRECTION ( 'NONE',  ( -0.005897974685767391929, 0.9999826067960413400, 0.000000000000000000 ) ) ;
#3291 = ORIENTED_EDGE ( 'NONE', *, *, #73, .T. ) ;
#3292 = EDGE_CURVE ( 'NONE', #14061, #1375, #14335, .T. ) ;
#3293 = LINE ( 'NONE', #13605, #1949 ) ;
#3294 = CARTESIAN_POINT ( 'NONE',  ( 8.171907405451781514, -55.68585955703573376, -1.912302604852146759 ) ) ;
#3295 = DIRECTION ( 'NONE',  ( -0.8746197071345571672, 0.4848096202550660205, 0.000000000000000000 ) ) ;
#3296 = DIRECTION ( 'NONE',  ( 0.000000000000000000, 0.000000000000000000, -1.000000000000000000 ) ) ;
#3297 = ORIENTED_EDGE ( 'NONE', *, *, #7639, .F. ) ;
#3298 = DIRECTION ( 'NONE',  ( 0.000000000000000000, 0.000000000000000000, -1.000000000000000000 ) ) ;
#3299 = ORIENTED_EDGE ( 'NONE', *, *, #1321, .T. ) ;
#3300 = DIRECTION ( 'NONE',  ( 0.000000000000000000, 0.000000000000000000, 1.000000000000000000 ) ) ;
#3301 = VERTEX_POINT ( 'NONE', #6394 ) ;
#3302 = EDGE_CURVE ( 'NONE', #369, #13514, #472, .T. ) ;
#3303 = EDGE_CURVE ( 'NONE', #7451, #4834, #6377, .T. ) ;
#3304 = CARTESIAN_POINT ( 'NONE',  ( 9.276697446006050285, -60.72048491829438888, -2.646952986712525657 ) ) ;
#3305 = PLANE ( 'NONE',  #12861 ) ;
#3306 = ORIENTED_EDGE ( 'NONE', *, *, #12717, .F. ) ;
#3307 = CARTESIAN_POINT ( 'NONE',  ( 8.782682478343074806, -56.07092277360308685, -2.830630916608713132 ) ) ;
#3308 = CYLINDRICAL_SURFACE ( 'NONE', #11587, 4.000000000000003553 ) ;
#3309 = EDGE_LOOP ( 'NONE', ( #1351, #5223, #4669, #8233, #9793, #14603, #6056 ) ) ;
#3310 = EDGE_CURVE ( 'NONE', #5867, #13804, #7330, .T. ) ;
#3311 = CARTESIAN_POINT ( 'NONE',  ( -0.9277479332649583021, -2.641590149077306826, 48.00000000000012079 ) ) ;
#3312 = CARTESIAN_POINT ( 'NONE',  ( 80.00000000000001421, -74.24929059928631148, 4.000000000000000000 ) ) ;
#3313 = CARTESIAN_POINT ( 'NONE',  ( 69.28051765693513175, -4.295678830383772961, 77.19766410831374515 ) ) ;
#3314 = CARTESIAN_POINT ( 'NONE',  ( 25.53134746123851784, -53.25924031079306786, 5.665074923594168865 ) ) ;
#3315 = CARTESIAN_POINT ( 'NONE',  ( 55.08546260466144417, 2.477934215446290445, 48.51982618741349285 ) ) ;
#3316 = ORIENTED_EDGE ( 'NONE', *, *, #10774, .T. ) ;
#3317 = CARTESIAN_POINT ( 'NONE',  ( 70.26445833701072274, -4.474174595298147317, 72.19766410831373094 ) ) ;
#3318 = EDGE_CURVE ( 'NONE', #3816, #14247, #11781, .T. ) ;
#3319 = ORIENTED_EDGE ( 'NONE', *, *, #9565, .T. ) ;
#3320 = DIRECTION ( 'NONE',  ( 0.000000000000000000, 0.000000000000000000, 1.000000000000000000 ) ) ;
#3321 = DIRECTION ( 'NONE',  ( 0.000000000000000000, 0.000000000000000000, -1.000000000000000000 ) ) ;
#3322 = CARTESIAN_POINT ( 'NONE',  ( -80.00000000000001421, -72.24929059928631148, -32.99999999999999289 ) ) ;
#3323 = CARTESIAN_POINT ( 'NONE',  ( 40.33162949095117966, 0.000000000000000000, 33.00000000000012790 ) ) ;
#3324 = VERTEX_POINT ( 'NONE', #13181 ) ;
#3325 = B_SPLINE_CURVE_WITH_KNOTS ( 'NONE', 3,
 ( #8008, #5789, #10320, #11621 ),
 .UNSPECIFIED., .F., .F.,
 ( 4, 4 ),
 ( 0.000000000000000000, 0.006642668954637878306 ),
 .UNSPECIFIED. ) ;
#3326 = LINE ( 'NONE', #778, #4567 ) ;
#3327 = DIRECTION ( 'NONE',  ( 0.000000000000000000, 0.000000000000000000, 1.000000000000000000 ) ) ;
#3328 = EDGE_CURVE ( 'NONE', #1460, #4646, #12250, .T. ) ;
#3329 = CARTESIAN_POINT ( 'NONE',  ( 58.00000000000000711, 2.256146146571122113, 36.00000000000012079 ) ) ;
#3330 = CARTESIAN_POINT ( 'NONE',  ( 13.41466460742225308, -66.31562986446988361, 3.513916789801492691 ) ) ;
#3331 = CARTESIAN_POINT ( 'NONE',  ( 8.821484763567294607, -57.33450387999030795, 2.749014434309869248 ) ) ;
#3332 = DIRECTION ( 'NONE',  ( -0.000000000000000000, 0.000000000000000000, -1.000000000000000000 ) ) ;
#3333 = VERTEX_POINT ( 'NONE', #10952 ) ;
#3334 = AXIS2_PLACEMENT_3D ( 'NONE', #7174, #8340, #1246 ) ;
#3335 = CARTESIAN_POINT ( 'NONE',  ( 31.88160194160486327, -62.60511169121411967, -2.715102820263733729 ) ) ;
#3336 = EDGE_LOOP ( 'NONE', ( #15179, #2343, #12257, #11325 ) ) ;
#3337 = CARTESIAN_POINT ( 'NONE',  ( 23.47858629692700205, -52.24929059928630437, -6.492462156583976629 ) ) ;
#3338 = CARTESIAN_POINT ( 'NONE',  ( 23.96426235118327597, -66.70789582472760060, 6.276998965480676596 ) ) ;
#3339 = ORIENTED_EDGE ( 'NONE', *, *, #10313, .F. ) ;
#3340 = DIRECTION ( 'NONE',  ( 0.000000000000000000, 0.000000000000000000, -1.000000000000000000 ) ) ;
#3341 = FACE_OUTER_BOUND ( 'NONE', #2167, .T. ) ;
#3342 = CARTESIAN_POINT ( 'NONE',  ( 58.00000000000000711, -2.249290599286309256, 61.61639468829817190 ) ) ;
#3343 = EDGE_CURVE ( 'NONE', #11072, #14286, #6612, .T. ) ;
#3344 = EDGE_CURVE ( 'NONE', #4786, #72, #8560, .T. ) ;
#3345 = AXIS2_PLACEMENT_3D ( 'NONE', #4197, #6441, #4125 ) ;
#3346 = CARTESIAN_POINT ( 'NONE',  ( 40.00000000000001421, -72.24929059928631148, -32.99999999999999289 ) ) ;
#3347 = CARTESIAN_POINT ( 'NONE',  ( 33.43599298439418277, -55.23669688164211777, -1.968664552513456956 ) ) ;
#3348 = CARTESIAN_POINT ( 'NONE',  ( 69.28051765693513175, -4.295678830383772961, 77.19766410831374515 ) ) ;
#3349 = DIRECTION ( 'NONE',  ( -0.000000000000000000, -0.000000000000000000, -1.000000000000000000 ) ) ;
#3350 = CARTESIAN_POINT ( 'NONE',  ( -9.456839514482961562, 2.659958822950721835, -48.50000000000012079 ) ) ;
#3351 = ADVANCED_FACE ( 'NONE', ( #1774 ), #8495, .T. ) ;
#3352 = VERTEX_POINT ( 'NONE', #3857 ) ;
#3353 = CARTESIAN_POINT ( 'NONE',  ( 17.70648456745510657, -67.68160391995883174, -6.249260988559856678 ) ) ;
#3354 = PRODUCT_DEFINITION_CONTEXT ( 'detailed design', #8324, 'design' ) ;
#3355 = VERTEX_POINT ( 'NONE', #13258 ) ;
#3356 = CARTESIAN_POINT ( 'NONE',  ( 32.95720782078544886, -57.08298494442341564, -2.747852995220870564 ) ) ;
#3357 = AXIS2_PLACEMENT_3D ( 'NONE', #11375, #10309, #5542 ) ;
#3358 = EDGE_LOOP ( 'NONE', ( #10086, #3124 ) ) ;
#3359 = LINE ( 'NONE', #1050, #495 ) ;
#3360 = CIRCLE ( 'NONE', #11449, 9.000000000000001776 ) ;
#3361 = DIRECTION ( 'NONE',  ( 0.000000000000000000, 0.000000000000000000, -1.000000000000000000 ) ) ;
#3362 = ADVANCED_FACE ( 'NONE', ( #10877 ), #1483, .T. ) ;
#3363 = CARTESIAN_POINT ( 'NONE',  ( 24.10826840236109803, -69.39711819508849544, -6.201611931792124111 ) ) ;
#3364 = ORIENTED_EDGE ( 'NONE', *, *, #14266, .T. ) ;
#3365 = AXIS2_PLACEMENT_3D ( 'NONE', #5286, #728, #10986 ) ;
#3366 =( GEOMETRIC_REPRESENTATION_CONTEXT ( 3 ) GLOBAL_UNCERTAINTY_ASSIGNED_CONTEXT ( ( #2586 ) ) GLOBAL_UNIT_ASSIGNED_CONTEXT ( ( #3939, #1571, #4958 ) ) REPRESENTATION_CONTEXT ( 'NONE', 'WORKASPACE' ) );
#3367 = EDGE_LOOP ( 'NONE', ( #1946, #1168, #13352, #2300 ) ) ;
#3368 = CIRCLE ( 'NONE', #13941, 0.7892041907098262810 ) ;
#3369 = CARTESIAN_POINT ( 'NONE',  ( 80.00000000000001421, -87.24929059928631148, 35.00000000000000000 ) ) ;
#3370 = CARTESIAN_POINT ( 'NONE',  ( 8.344481171119126017, -55.03829860714187561, -2.746682580607167079 ) ) ;
#3371 = DIRECTION ( 'NONE',  ( 0.000000000000000000, 0.000000000000000000, 1.000000000000000000 ) ) ;
#3372 = FACE_OUTER_BOUND ( 'NONE', #2382, .T. ) ;
#3373 = ORIENTED_EDGE ( 'NONE', *, *, #5898, .F. ) ;
#3374 = ORIENTED_EDGE ( 'NONE', *, *, #1518, .F. ) ;
#3375 = CARTESIAN_POINT ( 'NONE',  ( -21.85476584171713199, 5.329050157244537900, -57.50000000000012079 ) ) ;
#3376 = AXIS2_PLACEMENT_3D ( 'NONE', #2674, #9379, #7368 ) ;
#3377 = ORIENTED_EDGE ( 'NONE', *, *, #5054, .F. ) ;
#3378 = DIRECTION ( 'NONE',  ( -0.2245716668862467735, 0.9744202983869691970, 0.008523410314123130646 ) ) ;
#3379 = VERTEX_POINT ( 'NONE', #7483 ) ;
#3380 = VERTEX_POINT ( 'NONE', #1701 ) ;
#3381 = AXIS2_PLACEMENT_3D ( 'NONE', #3704, #14337, #12010 ) ;
#3382 = CARTESIAN_POINT ( 'NONE',  ( 48.84742675818896629, 2.824063592853376381, 81.40005259842790508 ) ) ;
#3383 = FACE_OUTER_BOUND ( 'NONE', #11906, .T. ) ;
#3384 = FACE_OUTER_BOUND ( 'NONE', #10476, .T. ) ;
#3385 = EDGE_CURVE ( 'NONE', #12875, #1311, #15226, .T. ) ;
#3386 = VERTEX_POINT ( 'NONE', #1562 ) ;
#3387 = VECTOR ( 'NONE', #8666, 1000.000000000000000 ) ;
#3388 = PLANE ( 'NONE',  #14203 ) ;
#3389 = CARTESIAN_POINT ( 'NONE',  ( -16.99999999999998579, -2.249290599286303927, -38.00000000000012079 ) ) ;
#3390 = ADVANCED_FACE ( 'NONE', ( #11164 ), #5168, .F. ) ;
#3391 = CARTESIAN_POINT ( 'NONE',  ( 68.02719294894561131, -7.807454411681058026, 71.19766410831374515 ) ) ;
#3392 = CARTESIAN_POINT ( 'NONE',  ( 24.31690506112493111, -73.00063092931685560, 6.088059227055016898 ) ) ;
#3393 = ORIENTED_EDGE ( 'NONE', *, *, #9079, .F. ) ;
#3394 = ADVANCED_FACE ( 'NONE', ( #4070 ), #8586, .T. ) ;
#3395 = DIRECTION ( 'NONE',  ( 0.000000000000000000, 0.000000000000000000, 1.000000000000000000 ) ) ;
#3396 = ORIENTED_EDGE ( 'NONE', *, *, #13536, .T. ) ;
#3397 = CARTESIAN_POINT ( 'NONE',  ( 54.86190032082818391, 1.721056973166403603, 62.84860122826521689 ) ) ;
#3398 = CARTESIAN_POINT ( 'NONE',  ( 0.000000000000000000, 21.75070940071325865, -33.00000000000012790 ) ) ;
#3399 = EDGE_CURVE ( 'NONE', #5759, #10066, #9805, .T. ) ;
#3400 = CIRCLE ( 'NONE', #892, 5.165819364273509073 ) ;
#3401 = CARTESIAN_POINT ( 'NONE',  ( 0.000000000000000000, 0.000000000000000000, 0.000000000000000000 ) ) ;
#3402 = CARTESIAN_POINT ( 'NONE',  ( 20.86173033120691045, -72.24929059928631148, 0.000000000000000000 ) ) ;
#3403 = DIRECTION ( 'NONE',  ( 1.000000000000000000, 0.000000000000000000, 0.000000000000000000 ) ) ;
#3404 = VERTEX_POINT ( 'NONE', #3932 ) ;
#3405 = ORIENTED_EDGE ( 'NONE', *, *, #13767, .F. ) ;
#3406 = VECTOR ( 'NONE', #1920, 1000.000000000000000 ) ;
#3407 = FACE_OUTER_BOUND ( 'NONE', #11403, .T. ) ;
#3408 = CARTESIAN_POINT ( 'NONE',  ( -16.99999999999998579, -2.249290599286305703, -115.4621125123531442 ) ) ;
#3409 = EDGE_CURVE ( 'NONE', #11544, #2824, #8451, .T. ) ;
#3410 = CARTESIAN_POINT ( 'NONE',  ( 93.56770215592470663, 21.75070940071356418, 33.00000000000012790 ) ) ;
#3411 = DIRECTION ( 'NONE',  ( -1.000000000000000000, 0.000000000000000000, -0.000000000000000000 ) ) ;
#3412 = CARTESIAN_POINT ( 'NONE',  ( -25.01741698508091005, -6.338425579613558014, -47.50000000000012079 ) ) ;
#3413 = CYLINDRICAL_SURFACE ( 'NONE', #6426, 9.000000000000001776 ) ;
#3414 = EDGE_CURVE ( 'NONE', #2105, #13865, #6856, .T. ) ;
#3415 = ORIENTED_EDGE ( 'NONE', *, *, #12379, .T. ) ;
#3416 = DIRECTION ( 'NONE',  ( 1.000000000000000000, -2.312964634635742895E-17, 0.000000000000000000 ) ) ;
#3417 = EDGE_CURVE ( 'NONE', #11292, #8222, #4227, .T. ) ;
#3418 = ORIENTED_EDGE ( 'NONE', *, *, #9385, .T. ) ;
#3419 = CARTESIAN_POINT ( 'NONE',  ( 8.317699921865331802, -55.12535711695123553, -1.983057912332487627 ) ) ;
#3420 = CARTESIAN_POINT ( 'NONE',  ( 63.00747169918385993, -1.516790343742004055, 60.61639468829817190 ) ) ;
#3421 = EDGE_LOOP ( 'NONE', ( #15097, #14300, #3236, #9525, #6608, #12971, #10003 ) ) ;
#3422 = DIRECTION ( 'NONE',  ( -0.000000000000000000, -0.000000000000000000, 1.000000000000000000 ) ) ;
#3423 = CARTESIAN_POINT ( 'NONE',  ( 63.36453054171181520, -0.8129776999179910701, 54.56811043785582882 ) ) ;
#3424 = CARTESIAN_POINT ( 'NONE',  ( 8.599030766203958009, -59.21224831720011395, -1.832439066039622144 ) ) ;
#3425 = AXIS2_PLACEMENT_3D ( 'NONE', #7024, #3563, #3411 ) ;
#3426 = VECTOR ( 'NONE', #12716, 1000.000000000000000 ) ;
#3427 = DIRECTION ( 'NONE',  ( 0.000000000000000000, -1.000000000000000000, -1.734723475976807094E-15 ) ) ;
#3428 = DIRECTION ( 'NONE',  ( 1.000000000000000000, 0.000000000000000000, 0.000000000000000000 ) ) ;
#3429 = DIRECTION ( 'NONE',  ( -1.000000000000000000, -8.673617379884035472E-17, 0.000000000000000000 ) ) ;
#3430 = ADVANCED_FACE ( 'NONE', ( #15013, #13544 ), #12703, .F. ) ;
#3431 = LINE ( 'NONE', #1037, #13598 ) ;
#3432 = FACE_OUTER_BOUND ( 'NONE', #2305, .T. ) ;
#3433 = EDGE_LOOP ( 'NONE', ( #11880, #2842, #1075, #5672 ) ) ;
#3434 = LINE ( 'NONE', #8289, #6808 ) ;
#3435 = EDGE_CURVE ( 'NONE', #538, #5126, #9087, .T. ) ;
#3436 = EDGE_CURVE ( 'NONE', #2361, #4051, #9080, .T. ) ;
#3437 = ORIENTED_EDGE ( 'NONE', *, *, #4601, .T. ) ;
#3438 = AXIS2_PLACEMENT_3D ( 'NONE', #3947, #15222, #10895 ) ;
#3439 = AXIS2_PLACEMENT_3D ( 'NONE', #4970, #9680, #6416 ) ;
#3440 = VERTEX_POINT ( 'NONE', #13776 ) ;
#3441 = DIRECTION ( 'NONE',  ( 0.000000000000000000, 1.000000000000000000, -0.000000000000000000 ) ) ;
#3442 = ORIENTED_EDGE ( 'NONE', *, *, #14415, .T. ) ;
#3443 = CARTESIAN_POINT ( 'NONE',  ( 58.00000000000000711, -2.249290599286307479, 139.1143251403882459 ) ) ;
#3444 = CARTESIAN_POINT ( 'NONE',  ( 58.00000000000000711, -2.249290599286307479, -33.00000000000012790 ) ) ;
#3445 = ORIENTED_EDGE ( 'NONE', *, *, #11700, .F. ) ;
#3446 = AXIS2_PLACEMENT_3D ( 'NONE', #10843, #4918, #1601 ) ;
#3447 = CARTESIAN_POINT ( 'NONE',  ( -24.80190064845255193, -6.760980556683136911, -48.50000000000010658 ) ) ;
#3448 = CARTESIAN_POINT ( 'NONE',  ( 9.167911396685996195, -53.68459816487493441, -2.283893849732906656 ) ) ;
#3449 = DIRECTION ( 'NONE',  ( 0.000000000000000000, -1.000000000000000000, 0.000000000000000000 ) ) ;
#3450 = CARTESIAN_POINT ( 'NONE',  ( -11.55417588973486609, -9.448993130794820061, 48.32458034489290100 ) ) ;
#3451 = EDGE_LOOP ( 'NONE', ( #2676, #5349, #13902, #11604 ) ) ;
#3452 = EDGE_CURVE ( 'NONE', #170, #7882, #763, .T. ) ;
#3453 = EDGE_CURVE ( 'NONE', #5614, #6214, #9170, .T. ) ;
#3454 = CYLINDRICAL_SURFACE ( 'NONE', #2166, 4.194885682587998765 ) ;
#3455 = B_SPLINE_CURVE_WITH_KNOTS ( 'NONE', 3,
 ( #1447, #5062, #144, #1217, #7373, #13074, #7220, #10610, #11832, #4990, #2532, #14152, #9767, #3901, #1526, #4833 ),
 .UNSPECIFIED., .F., .F.,
 ( 4, 2, 2, 2, 2, 2, 2, 4 ),
 ( 0.000000000000000000, 0.0003911934542035904491, 0.0007823869084071808982, 0.001173580362610771293, 0.001564773816814361796, 0.002347160725221542586, 0.002738354179425113791, 0.003129547633628685429 ),
 .UNSPECIFIED. ) ;
#3456 = EDGE_LOOP ( 'NONE', ( #265, #2688 ) ) ;
#3457 = CARTESIAN_POINT ( 'NONE',  ( 14.30638130925798812, -67.70775585802554986, 4.528449950254405110 ) ) ;
#3458 = ORIENTED_EDGE ( 'NONE', *, *, #14907, .F. ) ;
#3459 = ORIENTED_EDGE ( 'NONE', *, *, #5702, .F. ) ;
#3460 = VECTOR ( 'NONE', #13640, 1000.000000000000000 ) ;
#3461 = DIRECTION ( 'NONE',  ( -1.000000000000000000, -1.156482317317870492E-16, 0.000000000000000000 ) ) ;
#3462 = PLANE ( 'NONE',  #6224 ) ;
#3463 = ORIENTED_EDGE ( 'NONE', *, *, #1321, .F. ) ;
#3464 = CARTESIAN_POINT ( 'NONE',  ( -25.21252699837112132, -6.998437922861946880, -58.00000000000012079 ) ) ;
#3465 = LINE ( 'NONE', #1148, #770 ) ;
#3466 = ORIENTED_EDGE ( 'NONE', *, *, #449, .T. ) ;
#3467 = AXIS2_PLACEMENT_3D ( 'NONE', #7974, #4263, #13660 ) ;
#3468 = DIRECTION ( 'NONE',  ( -0.8656763553492632379, -0.5006040828730989878, 1.736819309459606431E-15 ) ) ;
#3469 = CARTESIAN_POINT ( 'NONE',  ( 64.30331578579614416, -11.82577336004862545, 72.28357345370125131 ) ) ;
#3470 = DIRECTION ( 'NONE',  ( 0.000000000000000000, 0.000000000000000000, 1.000000000000000000 ) ) ;
#3471 = DIRECTION ( 'NONE',  ( 5.551115123125787632E-16, 1.000000000000000000, -0.000000000000000000 ) ) ;
#3472 = ORIENTED_EDGE ( 'NONE', *, *, #5951, .F. ) ;
#3473 = LINE ( 'NONE', #10556, #3881 ) ;
#3474 = AXIS2_PLACEMENT_3D ( 'NONE', #4350, #12670, #12598 ) ;
#3475 = ORIENTED_EDGE ( 'NONE', *, *, #9530, .F. ) ;
#3476 = DIRECTION ( 'NONE',  ( 0.000000000000000000, 1.000000000000000000, 0.000000000000000000 ) ) ;
#3477 = CARTESIAN_POINT ( 'NONE',  ( 0.000000000000000000, 21.75070940071366365, -13.14990448602693007 ) ) ;
#3478 = CIRCLE ( 'NONE', #2740, 0.7892041907098262810 ) ;
#3479 = VECTOR ( 'NONE', #13091, 1000.000000000000000 ) ;
#3480 = DIRECTION ( 'NONE',  ( 0.000000000000000000, -1.000000000000000000, 0.000000000000000000 ) ) ;
#3481 = LINE ( 'NONE', #1088, #13098 ) ;
#3482 = ORIENTED_EDGE ( 'NONE', *, *, #8846, .T. ) ;
#3483 = CYLINDRICAL_SURFACE ( 'NONE', #5303, 4.999999999999997335 ) ;
#3484 = DIRECTION ( 'NONE',  ( -1.000000000000000000, 0.000000000000000000, 9.912705577010325549E-17 ) ) ;
#3485 = ADVANCED_FACE ( 'NONE', ( #13857 ), #7860, .F. ) ;
#3486 = VECTOR ( 'NONE', #3808, 1000.000000000000000 ) ;
#3488 = EDGE_CURVE ( 'NONE', #3759, #3805, #14242, .T. ) ;
#3487 = CARTESIAN_POINT ( 'NONE',  ( 58.00000000000000711, -2.249290599286309256, 61.61639468829817190 ) ) ;
#3489 = CARTESIAN_POINT ( 'NONE',  ( -11.83418063572647760, -2.249290599286303927, -57.50000000000012079 ) ) ;
#3490 = TOROIDAL_SURFACE ( 'NONE', #12090, 10.46463184759104870, 1.000000000000000000 ) ;
#3491 = CARTESIAN_POINT ( 'NONE',  ( -24.95893038578871881, -6.453098109823664608, -47.50000000000011369 ) ) ;
#3492 = ADVANCED_FACE ( 'NONE', ( #11383 ), #14617, .T. ) ;
#3493 = CARTESIAN_POINT ( 'NONE',  ( 52.94134894379979528, -2.395505968190773327, 62.84860122826521689 ) ) ;
#3494 = AXIS2_PLACEMENT_3D ( 'NONE', #8573, #12181, #484 ) ;
#3495 = VERTEX_POINT ( 'NONE', #11875 ) ;
#3496 = CARTESIAN_POINT ( 'NONE',  ( -3.190546569013415379, 0.8906624217387615339, 58.00000000000012079 ) ) ;
#3497 = ORIENTED_EDGE ( 'NONE', *, *, #11424, .F. ) ;
#3498 = CARTESIAN_POINT ( 'NONE',  ( 9.786677144408656659, -53.10505385066578299, -2.474491299097422825 ) ) ;
#3499 = CARTESIAN_POINT ( 'NONE',  ( 17.75919831123052717, -66.70789582472760060, 6.276998965480673043 ) ) ;
#3500 = ORIENTED_EDGE ( 'NONE', *, *, #4527, .T. ) ;
#3501 = VECTOR ( 'NONE', #4551, 1000.000000000000000 ) ;
#3502 = CARTESIAN_POINT ( 'NONE',  ( 80.00000000000001421, -74.24929059928631148, -32.00000000000000000 ) ) ;
#3503 = CYLINDRICAL_SURFACE ( 'NONE', #4597, 0.5000000000000004441 ) ;
#3504 = VECTOR ( 'NONE', #2422, 1000.000000000000000 ) ;
#3505 = ADVANCED_FACE ( 'NONE', ( #9807, #182 ), #14348, .F. ) ;
#3506 = AXIS2_PLACEMENT_3D ( 'NONE', #8845, #10008, #11079 ) ;
#3507 = ADVANCED_FACE ( 'NONE', ( #7257 ), #4876, .F. ) ;
#3508 = CARTESIAN_POINT ( 'NONE',  ( 8.201103799357262858, -57.48563641131178770, -1.816685854991388238 ) ) ;
#3509 = FACE_OUTER_BOUND ( 'NONE', #2666, .T. ) ;
#3510 = DIRECTION ( 'NONE',  ( 1.000000000000000000, 0.000000000000000000, 0.000000000000000000 ) ) ;
#3511 = CARTESIAN_POINT ( 'NONE',  ( -25.27051402993791029, -6.915952606384455414, 48.19241902544784750 ) ) ;
#3512 = DIRECTION ( 'NONE',  ( -1.000000000000000000, -0.000000000000000000, -0.000000000000000000 ) ) ;
#3513 = VECTOR ( 'NONE', #359, 1000.000000000000000 ) ;
#3514 = DIRECTION ( 'NONE',  ( -0.000000000000000000, -1.000000000000000000, -0.000000000000000000 ) ) ;
#3515 = EDGE_LOOP ( 'NONE', ( #11920, #3534 ) ) ;
#3516 = DIRECTION ( 'NONE',  ( 1.000000000000000000, 0.000000000000000000, 0.000000000000000000 ) ) ;
#3517 = PRODUCT_DEFINITION_CONTEXT ( 'detailed design', #5959, 'design' ) ;
#3518 = CIRCLE ( 'NONE', #6700, 9.000000000000001776 ) ;
#3519 = ORIENTED_EDGE ( 'NONE', *, *, #4576, .F. ) ;
#3520 = DIRECTION ( 'NONE',  ( 0.000000000000000000, 0.000000000000000000, 1.000000000000000000 ) ) ;
#3521 = ORIENTED_EDGE ( 'NONE', *, *, #12529, .F. ) ;
#3522 = VERTEX_POINT ( 'NONE', #7782 ) ;
#3523 = PLANE ( 'NONE',  #3013 ) ;
#3524 = CARTESIAN_POINT ( 'NONE',  ( 18.16985775135672654, -55.94205978621076980, -6.462225911923646926 ) ) ;
#3525 = CARTESIAN_POINT ( 'NONE',  ( 11.11753584644738346, -62.41236107492795071, -2.580051240451687988 ) ) ;
#3526 = CIRCLE ( 'NONE', #10157, 1.000000000000000222 ) ;
#3527 = EDGE_LOOP ( 'NONE', ( #8071, #1453, #1730, #11947 ) ) ;
#3528 = ADVANCED_FACE ( 'NONE', ( #12252 ), #6539, .F. ) ;
#3529 = VECTOR ( 'NONE', #2551, 1000.000000000000000 ) ;
#3530 = CARTESIAN_POINT ( 'NONE',  ( -24.54316048551696028, -7.158540021523408292, -48.50000000000011369 ) ) ;
#3531 = DIRECTION ( 'NONE',  ( 0.8746197071345569451, -0.4848096202550666312, 0.000000000000000000 ) ) ;
#3532 = CARTESIAN_POINT ( 'NONE',  ( -3.999999999999976019, -69.24929059928631148, -32.99999999999999289 ) ) ;
#3533 = EDGE_LOOP ( 'NONE', ( #13004, #3810, #10052, #7458 ) ) ;
#3534 = ORIENTED_EDGE ( 'NONE', *, *, #11664, .T. ) ;
#3535 = ORIENTED_EDGE ( 'NONE', *, *, #14400, .T. ) ;
#3536 = CARTESIAN_POINT ( 'NONE',  ( 9.984269850081815889, -60.50127194134182673, -2.962969586007857092 ) ) ;
#3537 = ORIENTED_EDGE ( 'NONE', *, *, #6762, .T. ) ;
#3538 = ORIENTED_EDGE ( 'NONE', *, *, #5966, .F. ) ;
#3539 = VECTOR ( 'NONE', #11207, 1000.000000000000000 ) ;
#3540 = FACE_OUTER_BOUND ( 'NONE', #7300, .T. ) ;
#3541 = DIRECTION ( 'NONE',  ( 0.000000000000000000, -0.000000000000000000, 1.000000000000000000 ) ) ;
#3542 = CARTESIAN_POINT ( 'NONE',  ( 20.86173033120691045, -82.24929059928629727, 3.999999999999999112 ) ) ;
#3543 = CARTESIAN_POINT ( 'NONE',  ( 70.25075679858845490, -4.321368936292105722, 72.19766410831378778 ) ) ;
#3544 = ORIENTED_EDGE ( 'NONE', *, *, #7499, .T. ) ;
#3545 = ADVANCED_FACE ( 'NONE', ( #11236 ), #7841, .T. ) ;
#3546 = DIRECTION ( 'NONE',  ( 0.000000000000000000, 1.000000000000000000, 0.000000000000000000 ) ) ;
#3547 = CARTESIAN_POINT ( 'NONE',  ( 53.11142512232702018, -3.558169932106523881, 48.51982618741349285 ) ) ;
#3548 = FACE_OUTER_BOUND ( 'NONE', #2642, .T. ) ;
#3549 = DIRECTION ( 'NONE',  ( -0.000000000000000000, -0.000000000000000000, -1.000000000000000000 ) ) ;
#3550 = ORIENTED_EDGE ( 'NONE', *, *, #8348, .T. ) ;
#3551 = CARTESIAN_POINT ( 'NONE',  ( 70.07302182237089028, -3.466915550704995574, 72.56882085266767035 ) ) ;
#3552 = ORIENTED_EDGE ( 'NONE', *, *, #7518, .T. ) ;
#3553 = FACE_OUTER_BOUND ( 'NONE', #2625, .T. ) ;
#3554 = CYLINDRICAL_SURFACE ( 'NONE', #6306, 0.7892041907098262810 ) ;
#3555 = CARTESIAN_POINT ( 'NONE',  ( 0.000000000000000000, 0.000000000000000000, 0.000000000000000000 ) ) ;
#3556 = CARTESIAN_POINT ( 'NONE',  ( -11.55417588973486609, -9.448993130794820061, -48.32458034489290100 ) ) ;
#3557 = CARTESIAN_POINT ( 'NONE',  ( 27.86173033120691045, -69.39711819508849544, 3.619682905202613377 ) ) ;
#3558 = ORIENTED_EDGE ( 'NONE', *, *, #4630, .T. ) ;
#3559 = EDGE_CURVE ( 'NONE', #14644, #7451, #9875, .T. ) ;
#3560 = CARTESIAN_POINT ( 'NONE',  ( -25.46282903980762669, -6.565599745187292946, 48.00000000000012079 ) ) ;
#3561 = CARTESIAN_POINT ( 'NONE',  ( 32.18160929697071992, -61.03551305047646736, -2.732671606847018264 ) ) ;
#3562 = DIRECTION ( 'NONE',  ( 1.000000000000000000, 0.000000000000000000, 0.000000000000000000 ) ) ;
#3563 = DIRECTION ( 'NONE',  ( 0.000000000000000000, 0.000000000000000000, -1.000000000000000000 ) ) ;
#3564 = CYLINDRICAL_SURFACE ( 'NONE', #7608, 3.999999999999999112 ) ;
#3565 = CARTESIAN_POINT ( 'NONE',  ( 109.8334623555409735, 21.75070940071366365, 139.1143251403882459 ) ) ;
#3566 = VERTEX_POINT ( 'NONE', #6397 ) ;
#3567 = CARTESIAN_POINT ( 'NONE',  ( 58.00000000000000711, -2.249290599286309256, 82.40005259842790508 ) ) ;
#3568 = EDGE_CURVE ( 'NONE', #322, #11132, #8854, .T. ) ;
#3569 = ORIENTED_EDGE ( 'NONE', *, *, #14929, .T. ) ;
#3570 = CARTESIAN_POINT ( 'NONE',  ( 8.127390121783262700, -55.95709369454765891, -1.884733065488557902 ) ) ;
#3571 = FACE_OUTER_BOUND ( 'NONE', #6982, .T. ) ;
#3572 = CARTESIAN_POINT ( 'NONE',  ( 112.9262740340969060, 23.25070940071369563, -33.00000000000012790 ) ) ;
#3573 = DIRECTION ( 'NONE',  ( -0.000000000000000000, -0.000000000000000000, -1.000000000000000000 ) ) ;
#3574 = DIRECTION ( 'NONE',  ( 0.000000000000000000, -0.000000000000000000, 1.000000000000000000 ) ) ;
#3575 = CARTESIAN_POINT ( 'NONE',  ( 14.38836832001927846, -69.49659648540917090, 4.497058153269694714 ) ) ;
#3576 = EDGE_CURVE ( 'NONE', #14799, #10038, #7555, .T. ) ;
#3577 = CARTESIAN_POINT ( 'NONE',  ( 38.50596956614688082, 13.12984319126714361, 91.03215601016300695 ) ) ;
#3578 = CARTESIAN_POINT ( 'NONE',  ( -25.15752072101212278, 2.619472661158555038, -47.50000000000012079 ) ) ;
#3579 = DIRECTION ( 'NONE',  ( 0.000000000000000000, 1.000000000000000000, 0.000000000000000000 ) ) ;
#3580 = CARTESIAN_POINT ( 'NONE',  ( 33.11767511809988207, -54.47948885957446663, 2.876625435111399121 ) ) ;
#3581 = EDGE_CURVE ( 'NONE', #446, #7966, #5251, .T. ) ;
#3582 = EDGE_LOOP ( 'NONE', ( #10686, #10805, #14708, #8367 ) ) ;
#3583 = ADVANCED_FACE ( 'NONE', ( #10554 ), #7862, .F. ) ;
#3584 = ADVANCED_FACE ( 'NONE', ( #1997 ), #6193, .F. ) ;
#3585 = LINE ( 'NONE', #14283, #3118 ) ;
#3586 = ORIENTED_EDGE ( 'NONE', *, *, #4794, .F. ) ;
#3587 = CARTESIAN_POINT ( 'NONE',  ( 12.03298173962126683, -53.28399145779480506, 4.141535524925028078 ) ) ;
#3588 = ORIENTED_EDGE ( 'NONE', *, *, #5413, .F. ) ;
#3589 = ORIENTED_EDGE ( 'NONE', *, *, #14866, .F. ) ;
#3590 = CARTESIAN_POINT ( 'NONE',  ( 65.33612023310359973, -11.06260784524912566, 77.14732870129599007 ) ) ;
#3591 = DIRECTION ( 'NONE',  ( 0.000000000000000000, 1.000000000000000000, -0.000000000000000000 ) ) ;
#3592 = ADVANCED_FACE ( 'NONE', ( #10240 ), #3235, .F. ) ;
#3593 = AXIS2_PLACEMENT_3D ( 'NONE', #5262, #9959, #2952 ) ;
#3594 = FACE_OUTER_BOUND ( 'NONE', #9135, .T. ) ;
#3595 = CARTESIAN_POINT ( 'NONE',  ( 8.753908754604131204, -54.21180406361235526, 2.945963350965704386 ) ) ;
#3596 = CARTESIAN_POINT ( 'NONE',  ( 8.821484763567292831, -57.33450387999030795, -2.749014434309867028 ) ) ;
#3597 = CARTESIAN_POINT ( 'NONE',  ( 10.00023835250150483, -61.42570632716525125, 2.132522520905371977 ) ) ;
#3598 = DIRECTION ( 'NONE',  ( -0.4848096202550659650, -0.8746197071345572782, 0.000000000000000000 ) ) ;
#3599 = VECTOR ( 'NONE', #14599, 1000.000000000000000 ) ;
#3600 = ORIENTED_EDGE ( 'NONE', *, *, #6884, .T. ) ;
#3601 = VERTEX_POINT ( 'NONE', #15015 ) ;
#3602 = CONICAL_SURFACE ( 'NONE', #7532, 2.524999999999999467, 0.7853981633973787790 ) ;
#3603 = CARTESIAN_POINT ( 'NONE',  ( -29.99999999999998224, -69.24929059928631148, -32.99999999999998579 ) ) ;
#3604 = ORIENTED_EDGE ( 'NONE', *, *, #13833, .F. ) ;
#3605 = FACE_OUTER_BOUND ( 'NONE', #10290, .T. ) ;
#3606 = ORIENTED_EDGE ( 'NONE', *, *, #9614, .F. ) ;
#3607 = CARTESIAN_POINT ( 'NONE',  ( -8.593267841128518825, 2.185894787177926624, 48.01308457333531265 ) ) ;
#3608 = EDGE_CURVE ( 'NONE', #5719, #5383, #4462, .T. ) ;
#3609 = ORIENTED_EDGE ( 'NONE', *, *, #11279, .T. ) ;
#3610 = CARTESIAN_POINT ( 'NONE',  ( -22.54958699671023581, 4.838095916862976686, -48.21133583021728697 ) ) ;
#3611 = DIRECTION ( 'NONE',  ( -0.000000000000000000, 0.000000000000000000, -1.000000000000000000 ) ) ;
#3612 = ORIENTED_EDGE ( 'NONE', *, *, #7311, .F. ) ;
#3613 = CIRCLE ( 'NONE', #12203, 0.7892041907098277242 ) ;
#3614 = CARTESIAN_POINT ( 'NONE',  ( 100.0000000000000284, 6.750709400713692965, -33.00000000000012790 ) ) ;
#3615 = CIRCLE ( 'NONE', #2385, 8.924024642120691908 ) ;
#3616 = CARTESIAN_POINT ( 'NONE',  ( 69.97972559857383601, -3.172990593254279457, 73.12044561456595204 ) ) ;
#3617 = ORIENTED_EDGE ( 'NONE', *, *, #6815, .T. ) ;
#3618 =( BOUNDED_SURFACE ( )  B_SPLINE_SURFACE ( 3, 2, ( 
 ( #12873, #10400, #6848 ),
 ( #8087, #9, #919 ),
 ( #5872, #12790, #3314 ),
 ( #10553, #15095, #4390 ) ),
 .UNSPECIFIED., .F., .F., .T. ) 
 B_SPLINE_SURFACE_WITH_KNOTS ( ( 4, 4 ),
 ( 3, 3 ),
 ( -3.469446951953614189E-18, 0.006683255761480933789 ),
 ( 0.000000000000000000, 1.000000000000000000 ),
 .UNSPECIFIED. ) 
 GEOMETRIC_REPRESENTATION_ITEM ( )  RATIONAL_B_SPLINE_SURFACE ( (
 ( 1.000000000000000000, 0.6947298545087535748, 1.000000000000000000),
 ( 1.000000000000000000, 0.6996284196041377967, 1.000000000000000000),
 ( 1.000000000000000000, 0.7035788727800780240, 1.000000000000000000),
 ( 1.000000000000000000, 0.7071067811865506814, 1.000000000000000000) ) ) 
 REPRESENTATION_ITEM ( '' )  SURFACE ( )  );
#3619 = FACE_OUTER_BOUND ( 'NONE', #11346, .T. ) ;
#3620 = CARTESIAN_POINT ( 'NONE',  ( -16.99999999999998579, -2.249290599286303927, 33.00000000000012790 ) ) ;
#3621 = CIRCLE ( 'NONE', #3853, 4.000000000000003553 ) ;
#3622 = LINE ( 'NONE', #13311, #11142 ) ;
#3623 = ORIENTED_EDGE ( 'NONE', *, *, #9810, .T. ) ;
#3624 = ORIENTED_EDGE ( 'NONE', *, *, #2656, .T. ) ;
#3625 = CARTESIAN_POINT ( 'NONE',  ( -23.00932074697458773, 4.484017154434125629, 48.14374739243680068 ) ) ;
#3626 = AXIS2_PLACEMENT_3D ( 'NONE', #8701, #14129, #13391 ) ;
#3627 = CIRCLE ( 'NONE', #1657, 11.46463184759105047 ) ;
#3628 = EDGE_CURVE ( 'NONE', #11798, #251, #12783, .T. ) ;
#3629 = VERTEX_POINT ( 'NONE', #3315 ) ;
#3630 = EDGE_CURVE ( 'NONE', #12374, #13354, #13273, .T. ) ;
#3631 = CYLINDRICAL_SURFACE ( 'NONE', #11840, 0.7892041907098262810 ) ;
#3632 = DIRECTION ( 'NONE',  ( 0.000000000000000000, 0.000000000000000000, -1.000000000000000000 ) ) ;
#3633 = ORIENTED_EDGE ( 'NONE', *, *, #5428, .T. ) ;
#3634 = ORIENTED_EDGE ( 'NONE', *, *, #4950, .F. ) ;
#3635 = DIRECTION ( 'NONE',  ( 1.000000000000000000, 0.000000000000000000, 0.000000000000000000 ) ) ;
#3636 = CYLINDRICAL_SURFACE ( 'NONE', #206, 2.499999999999995115 ) ;
#3637 = DIRECTION ( 'NONE',  ( -0.5006040828730974335, 0.8656763553492640151, 0.000000000000000000 ) ) ;
#3638 = AXIS2_PLACEMENT_3D ( 'NONE', #3749, #13145, #294 ) ;
#3639 = LINE ( 'NONE', #2330, #8988 ) ;
#3640 = CARTESIAN_POINT ( 'NONE',  ( 32.45002191802005598, -59.39772283578241030, -2.758706911752222712 ) ) ;
#3641 = VECTOR ( 'NONE', #4032, 999.9999999999998863 ) ;
#3642 = AXIS2_PLACEMENT_3D ( 'NONE', #9047, #13737, #8888 ) ;
#3643 = DIRECTION ( 'NONE',  ( -0.000000000000000000, 0.000000000000000000, -1.000000000000000000 ) ) ;
#3644 = CARTESIAN_POINT ( 'NONE',  ( 12.03298173962126150, -53.28399145779480506, -4.141535524925039624 ) ) ;
#3645 = CARTESIAN_POINT ( 'NONE',  ( 65.92402464212069901, -2.249290599286308368, 48.51982618741349285 ) ) ;
#3646 = CARTESIAN_POINT ( 'NONE',  ( 29.98342429842328727, -52.28415370497024384, -3.028416065278772162 ) ) ;
#3647 = VECTOR ( 'NONE', #4704, 1000.000000000000000 ) ;
#3648 = ORIENTED_EDGE ( 'NONE', *, *, #1567, .T. ) ;
#3649 = ADVANCED_FACE ( 'NONE', ( #12944 ), #9401, .T. ) ;
#3650 = LINE ( 'NONE', #6116, #5161 ) ;
#3651 = ADVANCED_FACE ( 'NONE', ( #6827 ), #12031, .T. ) ;
#3652 = ORIENTED_EDGE ( 'NONE', *, *, #8882, .F. ) ;
#3653 = PRODUCT_RELATED_PRODUCT_CATEGORY ( 'part', '', ( #675 ) ) ;
#3654 = PLANE ( 'NONE',  #6204 ) ;
#3655 = DIRECTION ( 'NONE',  ( -0.000000000000000000, 0.000000000000000000, -1.000000000000000000 ) ) ;
#3656 = AXIS2_PLACEMENT_3D ( 'NONE', #8168, #9399, #4459 ) ;
#3657 = DIRECTION ( 'NONE',  ( 0.000000000000000000, 1.000000000000000000, -0.000000000000000000 ) ) ;
#3658 = CARTESIAN_POINT ( 'NONE',  ( -16.99999999999998579, -2.249290599286303927, -48.00000000000012079 ) ) ;
#3659 = DIRECTION ( 'NONE',  ( 0.000000000000000000, 0.7071067811865965336, 0.7071067811864985009 ) ) ;
#3660 = CARTESIAN_POINT ( 'NONE',  ( 64.53644791741625397, -11.66848863668225711, 71.88150916912064758 ) ) ;
#3661 = CARTESIAN_POINT ( 'NONE',  ( 25.81270058232203013, 0.000000000000000000, 33.00000000000012790 ) ) ;
#3662 = CARTESIAN_POINT ( 'NONE',  ( -24.89252171451660445, -6.585377854361484040, 48.09696226170979827 ) ) ;
#3663 = CARTESIAN_POINT ( 'NONE',  ( 32.82016334605118857, -55.58238924893117172, 2.909054338253645344 ) ) ;
#3664 = ORIENTED_EDGE ( 'NONE', *, *, #13178, .T. ) ;
#3665 = DIRECTION ( 'NONE',  ( 1.000000000000000000, 0.000000000000000000, 0.000000000000000000 ) ) ;
#3666 = VERTEX_POINT ( 'NONE', #5685 ) ;
#3667 = DIRECTION ( 'NONE',  ( 0.000000000000000000, 0.000000000000000000, -1.000000000000000000 ) ) ;
#3668 = ORIENTED_EDGE ( 'NONE', *, *, #7814, .T. ) ;
#3669 = CARTESIAN_POINT ( 'NONE',  ( 65.52872014148834978, -10.89904965666429071, 77.19766409816131159 ) ) ;
#3670 = EDGE_CURVE ( 'NONE', #7624, #3759, #11359, .T. ) ;
#3671 = DIRECTION ( 'NONE',  ( 0.000000000000000000, 0.000000000000000000, 1.000000000000000000 ) ) ;
#3672 = LINE ( 'NONE', #4518, #8667 ) ;
#3673 = CARTESIAN_POINT ( 'NONE',  ( 9.845387176152206266, -54.14081474687885276, 3.331943113775061693 ) ) ;
#3674 = DIRECTION ( 'NONE',  ( -0.8908241094534361526, -0.4543483311474716957, 0.000000000000000000 ) ) ;
#3675 = CARTESIAN_POINT ( 'NONE',  ( 65.00000000000001421, -87.24929059928631148, 19.99999999999999645 ) ) ;
#3676 = AXIS2_PLACEMENT_3D ( 'NONE', #8702, #5248, #14621 ) ;
#3677 = EDGE_CURVE ( 'NONE', #3754, #788, #9224, .T. ) ;
#3678 = EDGE_LOOP ( 'NONE', ( #4914, #10504, #4931, #4425, #7013 ) ) ;
#3679 = ORIENTED_EDGE ( 'NONE', *, *, #691, .F. ) ;
#3680 = DIRECTION ( 'NONE',  ( 1.000000000000000000, -8.673617379884027583E-15, 0.000000000000000000 ) ) ;
#3681 = ORIENTED_EDGE ( 'NONE', *, *, #12056, .T. ) ;
#3682 = FACE_OUTER_BOUND ( 'NONE', #4540, .T. ) ;
#3683 = ORIENTED_EDGE ( 'NONE', *, *, #14758, .T. ) ;
#3684 = DIRECTION ( 'NONE',  ( 0.000000000000000000, 0.000000000000000000, -1.000000000000000000 ) ) ;
#3685 = ORIENTED_EDGE ( 'NONE', *, *, #6598, .F. ) ;
#3686 = DIRECTION ( 'NONE',  ( 0.000000000000000000, 0.000000000000000000, 1.000000000000000000 ) ) ;
#3687 = CARTESIAN_POINT ( 'NONE',  ( 0.5043391135745837195, 0.8906624217387615339, 48.50000000000012079 ) ) ;
#3688 = VERTEX_POINT ( 'NONE', #3065 ) ;
#3689 = EDGE_CURVE ( 'NONE', #550, #13470, #14991, .T. ) ;
#3690 = EDGE_CURVE ( 'NONE', #6772, #1096, #3293, .T. ) ;
#3691 = LINE ( 'NONE', #9555, #14057 ) ;
#3692 = DIRECTION ( 'NONE',  ( -1.000000000000000000, -0.000000000000000000, -0.000000000000000000 ) ) ;
#3693 = ORIENTED_EDGE ( 'NONE', *, *, #1457, .F. ) ;
#3694 = DIRECTION ( 'NONE',  ( -0.000000000000000000, -0.000000000000000000, -1.000000000000000000 ) ) ;
#3695 = CARTESIAN_POINT ( 'NONE',  ( 32.64893527110322680, -58.48797006926987763, 2.754379914540435959 ) ) ;
#3696 = DIRECTION ( 'NONE',  ( 0.000000000000000000, 0.000000000000000000, 1.000000000000000000 ) ) ;
#3697 = VERTEX_POINT ( 'NONE', #12766 ) ;
#3698 = CARTESIAN_POINT ( 'NONE',  ( -23.03920594196030791, 4.522656845271360915, 48.26696389624889605 ) ) ;
#3699 = VECTOR ( 'NONE', #15100, 1000.000000000000000 ) ;
#3700 = ORIENTED_EDGE ( 'NONE', *, *, #3194, .T. ) ;
#3701 = CARTESIAN_POINT ( 'NONE',  ( -25.01741698508091005, -6.338425579613558014, 47.50000000000012079 ) ) ;
#3702 = CARTESIAN_POINT ( 'NONE',  ( 20.86173033120691045, -52.24929059928630437, 0.000000000000000000 ) ) ;
#3703 = ORIENTED_EDGE ( 'NONE', *, *, #14732, .F. ) ;
#3704 = CARTESIAN_POINT ( 'NONE',  ( 23.36173033120691400, -85.24929059928631148, 6.000000000000001776 ) ) ;
#3705 = DIRECTION ( 'NONE',  ( -0.3020115420618322832, 0.1674077314120233917, -0.9384901064608587307 ) ) ;
#3706 = DIRECTION ( 'NONE',  ( 1.000000000000000000, 0.000000000000000000, 0.000000000000000000 ) ) ;
#3707 = AXIS2_PLACEMENT_3D ( 'NONE', #956, #5668, #4503 ) ;
#3708 = DIRECTION ( 'NONE',  ( 0.000000000000000000, 0.000000000000000000, 1.000000000000000000 ) ) ;
#3709 = DIRECTION ( 'NONE',  ( -0.000000000000000000, -0.000000000000000000, -1.000000000000000000 ) ) ;
#3710 = CARTESIAN_POINT ( 'NONE',  ( -28.95977857253358323, -8.587818791446789390, -57.50000000000012079 ) ) ;
#3711 = EDGE_CURVE ( 'NONE', #446, #5596, #11513, .T. ) ;
#3712 = CARTESIAN_POINT ( 'NONE',  ( 32.68132553305306232, -53.82357430177057012, 2.243931992452714130 ) ) ;
#3713 = CARTESIAN_POINT ( 'NONE',  ( 33.12442251017086647, -54.47420853489484216, -2.874994438546187858 ) ) ;
#3714 = AXIS2_PLACEMENT_3D ( 'NONE', #4192, #5522, #2205 ) ;
#3715 = AXIS2_PLACEMENT_3D ( 'NONE', #14322, #12157, #8829 ) ;
#3716 = CARTESIAN_POINT ( 'NONE',  ( -16.99999999999998579, -2.249290599286303927, 47.50000000000012079 ) ) ;
#3717 = ORIENTED_EDGE ( 'NONE', *, *, #7737, .F. ) ;
#3718 = DIRECTION ( 'NONE',  ( 0.000000000000000000, -1.000000000000000000, 0.000000000000000000 ) ) ;
#3719 = CARTESIAN_POINT ( 'NONE',  ( 84.72310019870096198, 29.52935533987996664, -33.00000000000013500 ) ) ;
#3720 = VERTEX_POINT ( 'NONE', #1973 ) ;
#3721 = CARTESIAN_POINT ( 'NONE',  ( 100.1541764164548880, 0.000000000000000000, 33.00000000000012790 ) ) ;
#3722 = DIRECTION ( 'NONE',  ( -0.000000000000000000, 0.000000000000000000, -1.000000000000000000 ) ) ;
#3723 = LINE ( 'NONE', #9670, #895 ) ;
#3724 = AXIS2_PLACEMENT_3D ( 'NONE', #4647, #1024, #12815 ) ;
#3725 = DIRECTION ( 'NONE',  ( 0.8656763553492639041, 0.5006040828730973224, 0.000000000000000000 ) ) ;
#3726 = CIRCLE ( 'NONE', #4205, 4.000000000000000000 ) ;
#3727 = EDGE_CURVE ( 'NONE', #8849, #7744, #3924, .T. ) ;
#3728 = LINE ( 'NONE', #14048, #4112 ) ;
#3729 = CARTESIAN_POINT ( 'NONE',  ( 58.00000000000000711, -2.249290599286309256, 47.51982618741348574 ) ) ;
#3730 = EDGE_CURVE ( 'NONE', #15028, #1311, #13679, .T. ) ;
#3731 = CARTESIAN_POINT ( 'NONE',  ( 30.88245120255916021, -52.50793004641701600, 3.755530264039013577 ) ) ;
#3732 = EDGE_LOOP ( 'NONE', ( #9194, #12086, #1206, #5379, #12814 ) ) ;
#3733 = LINE ( 'NONE', #6134, #12784 ) ;
#3734 = AXIS2_PLACEMENT_3D ( 'NONE', #2142, #2222, #3300 ) ;
#3735 = ORIENTED_EDGE ( 'NONE', *, *, #9530, .T. ) ;
#3736 = DIRECTION ( 'NONE',  ( 0.000000000000000000, 0.000000000000000000, 1.000000000000000000 ) ) ;
#3737 = VERTEX_POINT ( 'NONE', #12682 ) ;
#3738 = VERTEX_POINT ( 'NONE', #6599 ) ;
#3740 = ORIENTED_EDGE ( 'NONE', *, *, #4287, .F. ) ;
#3739 = CARTESIAN_POINT ( 'NONE',  ( 64.17477533520170141, -11.90904020766107863, 75.73640774255487429 ) ) ;
#3741 = CARTESIAN_POINT ( 'NONE',  ( 8.599030766203958009, -59.21224831720011395, 1.832439066039629916 ) ) ;
#3742 = CARTESIAN_POINT ( 'NONE',  ( 46.91810375148135392, 0.000000000000000000, -33.00000000000012790 ) ) ;
#3743 = ADVANCED_FACE ( 'NONE', ( #971 ), #12609, .F. ) ;
#3744 = AXIS2_PLACEMENT_3D ( 'NONE', #11819, #1278, #9687 ) ;
#3745 = DIRECTION ( 'NONE',  ( 0.000000000000000000, 0.000000000000000000, 1.000000000000000000 ) ) ;
#3746 = AXIS2_PLACEMENT_3D ( 'NONE', #2899, #588, #5289 ) ;
#3747 = CIRCLE ( 'NONE', #11857, 7.000000000000000000 ) ;
#3748 = CARTESIAN_POINT ( 'NONE',  ( 80.18290120114222930, 25.52935533987996664, -21.00807340887166674 ) ) ;
#3749 = CARTESIAN_POINT ( 'NONE',  ( 56.97758043373130477, 2.707118148285912795, 62.84860122826521689 ) ) ;
#3750 = CIRCLE ( 'NONE', #14808, 4.165819364273509962 ) ;
#3751 = ORIENTED_EDGE ( 'NONE', *, *, #5035, .F. ) ;
#3752 = VERTEX_POINT ( 'NONE', #4207 ) ;
#3753 = DIRECTION ( 'NONE',  ( 1.000000000000000000, 0.000000000000000000, 0.000000000000000000 ) ) ;
#3754 = VERTEX_POINT ( 'NONE', #4438 ) ;
#3755 = CARTESIAN_POINT ( 'NONE',  ( 53.27389963060701916, 0.6670697996139958175, 60.61639468829817190 ) ) ;
#3756 = VERTEX_POINT ( 'NONE', #12446 ) ;
#3757 = CARTESIAN_POINT ( 'NONE',  ( 30.26140529969011439, -61.79747627231876095, 3.500139319474480981 ) ) ;
#3758 = CIRCLE ( 'NONE', #12356, 4.000000000000003553 ) ;
#3759 = VERTEX_POINT ( 'NONE', #8911 ) ;
#3760 = AXIS2_PLACEMENT_3D ( 'NONE', #4600, #13992, #3295 ) ;
#3761 = CARTESIAN_POINT ( 'NONE',  ( 37.23881781239525424, 21.75070940071315562, 33.00000000000012790 ) ) ;
#3762 = CARTESIAN_POINT ( 'NONE',  ( -9.457494889590920550, -7.172893779636416056, 47.50000000000009237 ) ) ;
#3763 = VERTEX_POINT ( 'NONE', #1900 ) ;
#3764 = CIRCLE ( 'NONE', #1563, 1.000000000000007550 ) ;
#3765 = EDGE_CURVE ( 'NONE', #8760, #6117, #14050, .T. ) ;
#3766 = DIRECTION ( 'NONE',  ( 0.000000000000000000, 0.000000000000000000, 1.000000000000000000 ) ) ;
#3767 = CYLINDRICAL_SURFACE ( 'NONE', #7181, 2.000000000000000000 ) ;
#3768 = ORIENTED_EDGE ( 'NONE', *, *, #4630, .F. ) ;
#3769 = DIRECTION ( 'NONE',  ( -0.5006040828730773384, 0.8656763553492754504, 0.000000000000000000 ) ) ;
#3770 = DIRECTION ( 'NONE',  ( 0.000000000000000000, 0.000000000000000000, 1.000000000000000000 ) ) ;
#3771 = DIRECTION ( 'NONE',  ( 0.000000000000000000, 0.000000000000000000, 1.000000000000000000 ) ) ;
#3772 = EDGE_LOOP ( 'NONE', ( #7830, #6299, #2660, #10697, #1963, #9747 ) ) ;
#3773 = VECTOR ( 'NONE', #13976, 1000.000000000000114 ) ;
#3774 = CARTESIAN_POINT ( 'NONE',  ( -24.38033816570045076, 2.914516366099690448, 47.90685900410169040 ) ) ;
#3775 = AXIS2_PLACEMENT_3D ( 'NONE', #7091, #5010, #3771 ) ;
#3776 = ADVANCED_FACE ( 'NONE', ( #8981 ), #3138, .F. ) ;
#3777 = ADVANCED_FACE ( 'NONE', ( #6747 ), #9152, .T. ) ;
#3778 = ORIENTED_EDGE ( 'NONE', *, *, #13971, .T. ) ;
#3779 = LINE ( 'NONE', #4859, #11594 ) ;
#3780 = CARTESIAN_POINT ( 'NONE',  ( 69.46411667222970721, -2.361176089487651897, 72.68029919668498451 ) ) ;
#3781 = ORIENTED_EDGE ( 'NONE', *, *, #485, .F. ) ;
#3782 = SHAPE_DEFINITION_REPRESENTATION ( #6708, #8914 ) ;
#3783 = CARTESIAN_POINT ( 'NONE',  ( 8.599030766203956233, -59.21224831720010684, 1.832439066040435494 ) ) ;
#3784 = FACE_OUTER_BOUND ( 'NONE', #9288, .T. ) ;
#3785 = EDGE_CURVE ( 'NONE', #13205, #2898, #14729, .T. ) ;
#3786 = CARTESIAN_POINT ( 'NONE',  ( -9.198099345814858552, 2.262399347264687943, -48.43121057161710041 ) ) ;
#3787 = CARTESIAN_POINT ( 'NONE',  ( -24.96222495693456978, -7.431276100536581275, 58.00000000000012079 ) ) ;
#3789 = LINE ( 'NONE', #6188, #921 ) ;
#3788 =( REPRESENTATION_RELATIONSHIP ('NONE','NONE', #15125, #13539 ) REPRESENTATION_RELATIONSHIP_WITH_TRANSFORMATION ( #9074 )SHAPE_REPRESENTATION_RELATIONSHIP( ) );
#3790 = ADVANCED_FACE ( 'NONE', ( #8576 ), #14007, .F. ) ;
#3791 = CARTESIAN_POINT ( 'NONE',  ( 58.00000000000000711, -2.249290599286309256, 47.51982618741348574 ) ) ;
#3792 = CARTESIAN_POINT ( 'NONE',  ( 33.62180193043921861, -56.19320768388897847, 1.864142715824113283 ) ) ;
#3793 = CARTESIAN_POINT ( 'NONE',  ( 32.55528451253351108, -53.68423722363602479, -2.283982087544076389 ) ) ;
#3794 = FACE_OUTER_BOUND ( 'NONE', #2670, .T. ) ;
#3795 = ORIENTED_EDGE ( 'NONE', *, *, #1702, .F. ) ;
#3796 = CARTESIAN_POINT ( 'NONE',  ( 80.18290120114222930, 29.52935533987996664, -21.00807340887166674 ) ) ;
#3797 = DIRECTION ( 'NONE',  ( 1.000000000000000000, 8.270659117969274159E-16, 0.000000000000000000 ) ) ;
#3798 = DIRECTION ( 'NONE',  ( 1.000000000000000000, 0.000000000000000000, 0.000000000000000000 ) ) ;
#3799 = EDGE_CURVE ( 'NONE', #13514, #7142, #9341, .T. ) ;
#3800 = CARTESIAN_POINT ( 'NONE',  ( 69.32914122552278968, -4.026102965549716473, 76.25794738303314091 ) ) ;
#3801 = LINE ( 'NONE', #8505, #1019 ) ;
#3802 = CARTESIAN_POINT ( 'NONE',  ( 65.14877301755252859, -11.22304129159406116, 72.23267415556578896 ) ) ;
#3803 = DIRECTION ( 'NONE',  ( -1.000000000000000000, 0.000000000000000000, 0.000000000000000000 ) ) ;
#3804 = CARTESIAN_POINT ( 'NONE',  ( 29.70251902843242675, -52.24929059928631148, 4.175384597093458439 ) ) ;
#3805 = VERTEX_POINT ( 'NONE', #2369 ) ;
#3806 = DIRECTION ( 'NONE',  ( -0.4848096202550659650, -0.8746197071345572782, 0.000000000000000000 ) ) ;
#3807 = VERTEX_POINT ( 'NONE', #10603 ) ;
#3808 = DIRECTION ( 'NONE',  ( 1.000000000000000000, 0.000000000000000000, 0.000000000000000000 ) ) ;
#3809 = ORIENTED_EDGE ( 'NONE', *, *, #1479, .T. ) ;
#3810 = ORIENTED_EDGE ( 'NONE', *, *, #9661, .T. ) ;
#3811 = DIRECTION ( 'NONE',  ( 1.000000000000000000, 0.000000000000000000, 0.000000000000000000 ) ) ;
#3812 = DIRECTION ( 'NONE',  ( 0.3738365665314423159, 0.000000000000000000, -0.9274945937977119303 ) ) ;
#3813 = EDGE_CURVE ( 'NONE', #9928, #3922, #8645, .T. ) ;
#3814 = ADVANCED_FACE ( 'NONE', ( #10532 ), #13063, .T. ) ;
#3815 = FACE_OUTER_BOUND ( 'NONE', #1113, .T. ) ;
#3816 = VERTEX_POINT ( 'NONE', #6346 ) ;
#3817 = ORIENTED_EDGE ( 'NONE', *, *, #10104, .F. ) ;
#3818 = CARTESIAN_POINT ( 'NONE',  ( 8.471259741652538366, -54.75705460292326165, 2.044066819204477525 ) ) ;
#3819 = CARTESIAN_POINT ( 'NONE',  ( 100.1541764164548880, 0.000000000000000000, 139.1143251403882459 ) ) ;
#3820 = CARTESIAN_POINT ( 'NONE',  ( -12.09280073291247781, -82.24929059928629727, 11.78977872328357357 ) ) ;
#3821 = EDGE_LOOP ( 'NONE', ( #4973, #325, #13448, #12989 ) ) ;
#3822 = ORIENTED_EDGE ( 'NONE', *, *, #12731, .F. ) ;
#3823 = CARTESIAN_POINT ( 'NONE',  ( -28.70947653109703523, -9.020656969121422009, 57.50000000000012079 ) ) ;
#3824 = ORIENTED_EDGE ( 'NONE', *, *, #5099, .T. ) ;
#3825 = CARTESIAN_POINT ( 'NONE',  ( -22.41471376588497222, 4.941665658445489662, 48.26816462195809265 ) ) ;
#3826 = EDGE_LOOP ( 'NONE', ( #14610, #2703, #71 ) ) ;
#3827 = CARTESIAN_POINT ( 'NONE',  ( 29.96883933646702758, -63.18892729117397522, 3.546101824483956388 ) ) ;
#3828 = EDGE_CURVE ( 'NONE', #9158, #3629, #5198, .T. ) ;
#3829 = VECTOR ( 'NONE', #2846, 1000.000000000000000 ) ;
#3830 = ADVANCED_FACE ( 'NONE', ( #13277 ), #12119, .F. ) ;
#3831 = EDGE_LOOP ( 'NONE', ( #10010, #12858, #6498, #1677 ) ) ;
#3832 = LINE ( 'NONE', #2906, #1632 ) ;
#3833 = EDGE_LOOP ( 'NONE', ( #12228, #6363, #10709, #13289 ) ) ;
#3834 = CARTESIAN_POINT ( 'NONE',  ( 28.59185145675412443, -64.18054652438912910, -4.118450070759198667 ) ) ;
#3835 = DIRECTION ( 'NONE',  ( 0.000000000000000000, 0.000000000000000000, 1.000000000000000000 ) ) ;
#3836 = VERTEX_POINT ( 'NONE', #6209 ) ;
#3837 = CARTESIAN_POINT ( 'NONE',  ( -80.00000000000001421, -74.24929059928631148, 8.000000000000001776 ) ) ;
#3838 = LINE ( 'NONE', #13018, #4196 ) ;
#3839 = DIRECTION ( 'NONE',  ( -0.000000000000000000, -0.000000000000000000, 1.000000000000000000 ) ) ;
#3840 = ORIENTED_EDGE ( 'NONE', *, *, #6598, .T. ) ;
#3841 = CARTESIAN_POINT ( 'NONE',  ( -21.85476584171706449, 5.329050157244580532, 48.50000000000012079 ) ) ;
#3842 = ORIENTED_EDGE ( 'NONE', *, *, #2690, .F. ) ;
#3843 = ORIENTED_EDGE ( 'NONE', *, *, #8706, .T. ) ;
#3844 = CARTESIAN_POINT ( 'NONE',  ( -28.70947653109703168, -9.020656969121420232, 57.50000000000012079 ) ) ;
#3845 = VECTOR ( 'NONE', #14312, 1000.000000000000000 ) ;
#3846 = ORIENTED_EDGE ( 'NONE', *, *, #950, .T. ) ;
#3847 = AXIS2_PLACEMENT_3D ( 'NONE', #11592, #1052, #8226 ) ;
#3848 = CARTESIAN_POINT ( 'NONE',  ( 53.54504563787001814, -4.650271872399136086, 60.61639468829817190 ) ) ;
#3849 = ADVANCED_FACE ( 'NONE', ( #5844 ), #352, .F. ) ;
#3850 = DIRECTION ( 'NONE',  ( 0.000000000000000000, 1.000000000000000000, 4.625929269271485914E-16 ) ) ;
#3851 = CARTESIAN_POINT ( 'NONE',  ( -8.729485970062036415, 2.417371407811747197, -48.19241902544784750 ) ) ;
#3852 = DIRECTION ( 'NONE',  ( 0.000000000000000000, -1.000000000000000000, 0.000000000000000000 ) ) ;
#3853 = AXIS2_PLACEMENT_3D ( 'NONE', #14819, #6364, #11129 ) ;
#3854 = EDGE_CURVE ( 'NONE', #2280, #3040, #11678, .T. ) ;
#3855 = ADVANCED_FACE ( 'NONE', ( #7349, #1577 ), #5042, .F. ) ;
#3856 = CARTESIAN_POINT ( 'NONE',  ( 32.72879314807957485, -60.25563941105167487, 1.887923216546060212 ) ) ;
#3857 = CARTESIAN_POINT ( 'NONE',  ( 55.08546260466144417, 2.477934215446290445, 60.61639468829817190 ) ) ;
#3858 = VECTOR ( 'NONE', #8478, 1000.000000000000000 ) ;
#3859 = CARTESIAN_POINT ( 'NONE',  ( 29.35555050496136431, -52.24929059928631148, 3.199931146564417350 ) ) ;
#3860 = CARTESIAN_POINT ( 'NONE',  ( 33.03498543261559206, -54.32282595323827934, -2.125007313488010308 ) ) ;
#3861 = CIRCLE ( 'NONE', #10259, 10.46463184759104692 ) ;
#3862 = ADVANCED_FACE ( 'NONE', ( #6275 ), #12066, .F. ) ;
#3863 = ADVANCED_FACE ( 'NONE', ( #11322 ), #786, .T. ) ;
#3864 = DIRECTION ( 'NONE',  ( 0.000000000000000000, 1.000000000000000000, 0.000000000000000000 ) ) ;
#3865 = ORIENTED_EDGE ( 'NONE', *, *, #6225, .T. ) ;
#3866 = FILL_AREA_STYLE_COLOUR ( '', #4464 ) ;
#3867 = CARTESIAN_POINT ( 'NONE',  ( 33.38971410812750662, -58.06117559053650723, -1.821720188305476773 ) ) ;
#3868 = AXIS2_PLACEMENT_3D ( 'NONE', #6890, #4265, #11580 ) ;
#3869 = PRODUCT_DEFINITION_FORMATION_WITH_SPECIFIED_SOURCE ( 'ANY', '', #2889, .NOT_KNOWN. ) ;
#3870 = DIRECTION ( 'NONE',  ( 0.8420378618367728718, 0.5394184268574404584, -0.000000000000000000 ) ) ;
#3871 = FACE_OUTER_BOUND ( 'NONE', #8927, .T. ) ;
#3872 = VECTOR ( 'NONE', #4501, 1000.000000000000000 ) ;
#3873 = EDGE_CURVE ( 'NONE', #5614, #8184, #14871, .T. ) ;
#3874 = AXIS2_PLACEMENT_3D ( 'NONE', #2705, #7699, #8844 ) ;
#3875 = CARTESIAN_POINT ( 'NONE',  ( 69.45987574584773938, -2.588318118538463608, 76.22979495466215383 ) ) ;
#3876 = CARTESIAN_POINT ( 'NONE',  ( 64.29082196272626959, -11.83396660969246561, 72.31276519526322488 ) ) ;
#3877 = ADVANCED_FACE ( 'NONE', ( #13723 ), #3178, .F. ) ;
#3878 = ADVANCED_FACE ( 'NONE', ( #12569 ), #10109, .T. ) ;
#3879 = CARTESIAN_POINT ( 'NONE',  ( -16.99999999999998579, -2.249290599286303927, -50.50000000000012079 ) ) ;
#3880 = CARTESIAN_POINT ( 'NONE',  ( 8.948129010634172431, -57.91122518709823908, -2.751677560524413035 ) ) ;
#3881 = VECTOR ( 'NONE', #6935, 1000.000000000000000 ) ;
#3882 = VECTOR ( 'NONE', #14886, 1000.000000000000000 ) ;
#3883 = ORIENTED_EDGE ( 'NONE', *, *, #2263, .T. ) ;
#3884 = FACE_OUTER_BOUND ( 'NONE', #4685, .T. ) ;
#3885 = EDGE_LOOP ( 'NONE', ( #3768, #12110, #1367, #5122 ) ) ;
#3886 = CARTESIAN_POINT ( 'NONE',  ( 24.10826840236109803, -69.39711819508849544, -6.201611931792124111 ) ) ;
#3887 = DIRECTION ( 'NONE',  ( 1.000000000000000000, 0.000000000000000000, 0.000000000000000000 ) ) ;
#3888 = ORIENTED_EDGE ( 'NONE', *, *, #13193, .T. ) ;
#3890 = ORIENTED_EDGE ( 'NONE', *, *, #14215, .T. ) ;
#3889 = CARTESIAN_POINT ( 'NONE',  ( -12.14523415828296216, -9.827631355817223024, 48.50000000000012079 ) ) ;
#3891 = CARTESIAN_POINT ( 'NONE',  ( 20.86173033120691045, -72.24929059928631148, 0.000000000000000000 ) ) ;
#3892 = DIRECTION ( 'NONE',  ( 1.000000000000000000, 0.000000000000000000, 0.000000000000000000 ) ) ;
#3893 = EDGE_LOOP ( 'NONE', ( #130, #380, #11295, #4351 ) ) ;
#3894 = EDGE_LOOP ( 'NONE', ( #1837, #2359, #11373, #7836 ) ) ;
#3895 = PLANE ( 'NONE',  #13847 ) ;
#3896 = EDGE_CURVE ( 'NONE', #3836, #10222, #6872, .T. ) ;
#3897 = ADVANCED_FACE ( 'NONE', ( #4091 ), #13642, .F. ) ;
#3898 = CARTESIAN_POINT ( 'NONE',  ( 59.00001739350650354, 10.75070940071368852, 33.00000000000012790 ) ) ;
#3899 = VERTEX_POINT ( 'NONE', #6413 ) ;
#3900 = ORIENTED_EDGE ( 'NONE', *, *, #6796, .F. ) ;
#3901 = CARTESIAN_POINT ( 'NONE',  ( 64.12508379658279978, -11.94061857445316477, 75.45956441370945811 ) ) ;
#3902 = ORIENTED_EDGE ( 'NONE', *, *, #12062, .F. ) ;
#3903 = DIRECTION ( 'NONE',  ( -1.000000000000000000, 0.000000000000000000, -0.000000000000000000 ) ) ;
#3904 = VERTEX_POINT ( 'NONE', #5267 ) ;
#3905 = CARTESIAN_POINT ( 'NONE',  ( 29.10765984106813420, -64.50532980541188977, 3.862852061917652513 ) ) ;
#3906 = ORIENTED_EDGE ( 'NONE', *, *, #11823, .T. ) ;
#3907 = DIRECTION ( 'NONE',  ( -0.000000000000000000, -0.000000000000000000, -1.000000000000000000 ) ) ;
#3908 = DIRECTION ( 'NONE',  ( 1.000000000000000000, 0.000000000000000000, 0.000000000000000000 ) ) ;
#3909 = ORIENTED_EDGE ( 'NONE', *, *, #13049, .T. ) ;
#3910 = CARTESIAN_POINT ( 'NONE',  ( 29.24098086411812147, -64.27177309650900838, -3.135762038892989878 ) ) ;
#3911 = ORIENTED_EDGE ( 'NONE', *, *, #9809, .T. ) ;
#3912 = VECTOR ( 'NONE', #14485, 1000.000000000000000 ) ;
#3913 = CIRCLE ( 'NONE', #13490, 8.500000000000000000 ) ;
#3914 = EDGE_CURVE ( 'NONE', #13135, #5290, #9962, .T. ) ;
#3915 = LINE ( 'NONE', #13309, #4596 ) ;
#3916 = CARTESIAN_POINT ( 'NONE',  ( 63.55816381239476698, 7.777902349659290948, 82.40005259842790508 ) ) ;
#3917 = EDGE_CURVE ( 'NONE', #6801, #6058, #8794, .T. ) ;
#3918 = DIRECTION ( 'NONE',  ( 1.000000000000000000, 0.000000000000000000, 0.000000000000000000 ) ) ;
#3919 = ORIENTED_EDGE ( 'NONE', *, *, #5704, .T. ) ;
#3920 = CARTESIAN_POINT ( 'NONE',  ( -24.14404371603619381, 3.605862562765568491, 48.08251050686933326 ) ) ;
#3921 = VERTEX_POINT ( 'NONE', #2255 ) ;
#3922 = VERTEX_POINT ( 'NONE', #13878 ) ;
#3923 = DIRECTION ( 'NONE',  ( 1.000000000000000000, 0.000000000000000000, 0.000000000000000000 ) ) ;
#3924 = CIRCLE ( 'NONE', #718, 4.194885682587998765 ) ;
#3925 = VERTEX_POINT ( 'NONE', #8270 ) ;
#3926 = CONTEXT_DEPENDENT_SHAPE_REPRESENTATION ( #11653, #7409 ) ;
#3927 = DIRECTION ( 'NONE',  ( -0.9528381992908617759, -0.3034787735116703522, 0.000000000000000000 ) ) ;
#3928 = LINE ( 'NONE', #12242, #1539 ) ;
#3929 = B_SPLINE_CURVE_WITH_KNOTS ( 'NONE', 3,
 ( #6271, #1642, #9817, #14500, #5038, #3876, #9671, #14206, #3660, #8640, #13048, #10732, #7422, #8358, #3943, #7267, #195, #13341 ),
 .UNSPECIFIED., .F., .F.,
 ( 4, 2, 2, 2, 2, 2, 2, 2, 4 ),
 ( 0.000000000000000000, 0.0003958370570530560847, 0.0007916741141061121693, 0.001187511171159168254, 0.001583348228212224339, 0.001979185285265280640, 0.002375022342318336508, 0.002770859399371392376, 0.003166696456424448677 ),
 .UNSPECIFIED. ) ;
#3930 = DIRECTION ( 'NONE',  ( -1.000000000000000000, 9.251858538542971581E-17, 0.000000000000000000 ) ) ;
#3931 = CARTESIAN_POINT ( 'NONE',  ( 13.24997490312535753, -58.78531205390407877, 4.199849437504418859 ) ) ;
#3932 = CARTESIAN_POINT ( 'NONE',  ( 54.85055839958032209, 23.25070940071368852, -33.00000000000012790 ) ) ;
#3933 = CARTESIAN_POINT ( 'NONE',  ( 64.64681977576810823, -12.79380737173441140, 73.19766410831374515 ) ) ;
#3934 = CARTESIAN_POINT ( 'NONE',  ( 33.31490201906242277, -54.89597349494514589, -2.779010397565622625 ) ) ;
#3935 = CARTESIAN_POINT ( 'NONE',  ( -24.96222495693456978, -7.431276100536581275, 57.50000000000012079 ) ) ;
#3936 = ORIENTED_EDGE ( 'NONE', *, *, #14969, .F. ) ;
#3937 = CARTESIAN_POINT ( 'NONE',  ( -16.99999999999998579, -2.249290599286303927, 38.00000000000012079 ) ) ;
#3938 = CARTESIAN_POINT ( 'NONE',  ( 80.00000000000001421, -72.24929059928631148, -32.99999999999999289 ) ) ;
#3939 =( LENGTH_UNIT ( ) NAMED_UNIT ( * ) SI_UNIT ( .MILLI., .METRE. ) );
#3940 = CARTESIAN_POINT ( 'NONE',  ( 60.40269930420516431, 2.204737408716291647, 48.51982618741349285 ) ) ;
#3941 = ADVANCED_FACE ( 'NONE', ( #8029 ), #5705, .T. ) ;
#3942 = CARTESIAN_POINT ( 'NONE',  ( 53.04398595309534414, -1.224959495890951100, 48.51982618741349285 ) ) ;
#3943 = CARTESIAN_POINT ( 'NONE',  ( 65.32355913535712943, -11.07082656745060234, 71.26415692744444641 ) ) ;
#3944 = EDGE_CURVE ( 'NONE', #9712, #2379, #9877, .T. ) ;
#3945 = ADVANCED_FACE ( 'NONE', ( #12894 ), #12730, .T. ) ;
#3946 = DIRECTION ( 'NONE',  ( -1.000000000000000000, 0.000000000000000000, -0.000000000000000000 ) ) ;
#3947 = CARTESIAN_POINT ( 'NONE',  ( -16.99999999999998579, -2.249290599286303927, 38.00000000000012079 ) ) ;
#3948 = VECTOR ( 'NONE', #13738, 1000.000000000000000 ) ;
#3949 = ORIENTED_EDGE ( 'NONE', *, *, #3914, .T. ) ;
#3950 = CARTESIAN_POINT ( 'NONE',  ( 28.02673944706192088, -65.45069003752192316, -4.122770147305073074 ) ) ;
#3951 = ORIENTED_EDGE ( 'NONE', *, *, #8899, .F. ) ;
#3952 = EDGE_CURVE ( 'NONE', #10066, #2563, #14113, .T. ) ;
#3953 = DIRECTION ( 'NONE',  ( -0.000000000000000000, 1.000000000000000000, -0.000000000000000000 ) ) ;
#3954 = DIRECTION ( 'NONE',  ( -0.000000000000000000, -0.000000000000000000, -1.000000000000000000 ) ) ;
#3955 = ADVANCED_FACE ( 'NONE', ( #14955 ), #3413, .T. ) ;
#3956 = ORIENTED_EDGE ( 'NONE', *, *, #13284, .F. ) ;
#3957 = CIRCLE ( 'NONE', #4203, 0.9999999999999980016 ) ;
#3959 = ORIENTED_EDGE ( 'NONE', *, *, #13050, .T. ) ;
#3958 = CARTESIAN_POINT ( 'NONE',  ( 57.26556849154462725, -7.256479411572841265, 60.61639468829817190 ) ) ;
#3960 = DIRECTION ( 'NONE',  ( 0.5394184268574402363, -0.8420378618367729828, 0.000000000000000000 ) ) ;
#3961 = AXIS2_PLACEMENT_3D ( 'NONE', #10487, #12804, #2249 ) ;
#3962 = CYLINDRICAL_SURFACE ( 'NONE', #1794, 4.665819364273509073 ) ;
#3963 = DIRECTION ( 'NONE',  ( -0.8746197071345569451, 0.4848096202550666312, 0.000000000000000000 ) ) ;
#3964 = CARTESIAN_POINT ( 'NONE',  ( 80.18290120114222930, 29.52935533987996664, -21.00807340887166674 ) ) ;
#3965 = CIRCLE ( 'NONE', #530, 10.00000000000000000 ) ;
#3966 = AXIS2_PLACEMENT_3D ( 'NONE', #8979, #1897, #14901 ) ;
#3967 = CARTESIAN_POINT ( 'NONE',  ( 65.00000000000001421, -85.24929059928631148, 19.99999999999999645 ) ) ;
#3968 = VERTEX_POINT ( 'NONE', #8110 ) ;
#3969 = VECTOR ( 'NONE', #11032, 1000.000000000000000 ) ;
#3970 = EDGE_LOOP ( 'NONE', ( #14521, #4201, #1735, #2671 ) ) ;
#3971 = LINE ( 'NONE', #1596, #7794 ) ;
#3972 = VERTEX_POINT ( 'NONE', #1095 ) ;
#3973 = DIRECTION ( 'NONE',  ( 0.000000000000000000, 0.000000000000000000, -1.000000000000000000 ) ) ;
#3974 = ORIENTED_EDGE ( 'NONE', *, *, #7880, .F. ) ;
#3975 = CARTESIAN_POINT ( 'NONE',  ( 65.13162939602317181, -11.91918766459985157, 75.19766410831374515 ) ) ;
#3976 = VERTEX_POINT ( 'NONE', #2179 ) ;
#3977 = CIRCLE ( 'NONE', #7678, 5.496540510819677650 ) ;
#3978 = LINE ( 'NONE', #1681, #6068 ) ;
#3979 = CARTESIAN_POINT ( 'NONE',  ( 65.13162939602317181, -11.91918766459985157, 72.19766410831374515 ) ) ;
#3980 = ORIENTED_EDGE ( 'NONE', *, *, #7921, .F. ) ;
#3981 = AXIS2_PLACEMENT_3D ( 'NONE', #12190, #3954, #3887 ) ;
#3982 = ADVANCED_FACE ( 'NONE', ( #13795 ), #4709, .F. ) ;
#3983 = CIRCLE ( 'NONE', #11610, 0.9999999999999951150 ) ;
#3984 = CARTESIAN_POINT ( 'NONE',  ( -12.99999999999998757, -2.249290599286303927, -47.31370849898487307 ) ) ;
#3985 = ORIENTED_EDGE ( 'NONE', *, *, #3452, .T. ) ;
#3986 = VECTOR ( 'NONE', #15219, 1000.000000000000000 ) ;
#3987 = CARTESIAN_POINT ( 'NONE',  ( 105.5545870572953930, -1.749290599286305259, 13.14990448602692474 ) ) ;
#3988 = CARTESIAN_POINT ( 'NONE',  ( -11.83418063572647760, -2.249290599286303927, -58.00000000000012079 ) ) ;
#3989 = DIRECTION ( 'NONE',  ( -0.000000000000000000, -0.000000000000000000, -1.000000000000000000 ) ) ;
#3990 = ORIENTED_EDGE ( 'NONE', *, *, #4861, .F. ) ;
#3991 = AXIS2_PLACEMENT_3D ( 'NONE', #6880, #3270, #4258 ) ;
#3992 = DIRECTION ( 'NONE',  ( 0.000000000000000000, 1.000000000000000000, 0.000000000000000000 ) ) ;
#3993 = ORIENTED_EDGE ( 'NONE', *, *, #2923, .T. ) ;
#3994 = ORIENTED_EDGE ( 'NONE', *, *, #9732, .F. ) ;
#3995 = CIRCLE ( 'NONE', #9672, 0.5000000000000004441 ) ;
#3996 = CARTESIAN_POINT ( 'NONE',  ( 80.00000000000001421, -76.24929059928631148, -6.000000000000000000 ) ) ;
#3997 = APPLICATION_PROTOCOL_DEFINITION ( 'draft international standard', 'automotive_design', 1998, #8511 ) ;
#3998 = DIRECTION ( 'NONE',  ( -0.000000000000000000, -0.000000000000000000, -1.000000000000000000 ) ) ;
#3999 = LINE ( 'NONE', #14693, #66 ) ;
#4000 = EDGE_CURVE ( 'NONE', #11210, #8448, #4643, .T. ) ;
#4001 = DIRECTION ( 'NONE',  ( -0.8571673007072465600, -0.5150380749015093240, 0.000000000000000000 ) ) ;
#4002 = CARTESIAN_POINT ( 'NONE',  ( 7.495397352420198445, -51.17708206447213115, 2.732753929628628065 ) ) ;
#4003 = FACE_OUTER_BOUND ( 'NONE', #12412, .T. ) ;
#4004 = CIRCLE ( 'NONE', #9679, 0.7892041907098262810 ) ;
#4005 = DIRECTION ( 'NONE',  ( -0.000000000000000000, -0.000000000000000000, -1.000000000000000000 ) ) ;
#4006 = AXIS2_PLACEMENT_3D ( 'NONE', #93, #2617, #4783 ) ;
#4007 = CARTESIAN_POINT ( 'NONE',  ( -8.982583014919022446, 1.839844381040865118, 47.50000000000012079 ) ) ;
#4008 = CARTESIAN_POINT ( 'NONE',  ( 12.61580082134606684, -64.50532980541187555, -3.862852061920813984 ) ) ;
#4009 =( BOUNDED_SURFACE ( )  B_SPLINE_SURFACE ( 3, 2, ( 
 ( #11444, #680, #1839 ),
 ( #13695, #9164, #13617 ),
 ( #5467, #10160, #2146 ),
 ( #3151, #3304, #7851 ),
 ( #12543, #4451, #911 ),
 ( #1988, #6688, #7997 ) ),
 .UNSPECIFIED., .F., .F., .F. ) 
 B_SPLINE_SURFACE_WITH_KNOTS ( ( 4, 2, 4 ),
 ( 3, 3 ),
 ( 1.084202172485504434E-19, 0.001005789800061011787, 0.002011579600122023574 ),
 ( 0.000000000000000000, 1.000000000000000000 ),
 .UNSPECIFIED. ) 
 GEOMETRIC_REPRESENTATION_ITEM ( )  RATIONAL_B_SPLINE_SURFACE ( (
 ( 1.000000000000000000, 0.8308543624379425285, 1.000000000000000000),
 ( 1.000000000000000000, 0.8317114229140971648, 1.000000000000000000),
 ( 1.000000000000000000, 0.8301458553070009128, 1.000000000000000000),
 ( 1.000000000000000000, 0.8215594255314535577, 1.000000000000000000),
 ( 1.000000000000000000, 0.8147253674585736016, 1.000000000000000000),
 ( 1.000000000000000000, 0.8053615646146359275, 1.000000000000000000) ) ) 
 REPRESENTATION_ITEM ( '' )  SURFACE ( )  );
#4010 = DIRECTION ( 'NONE',  ( -0.000000000000000000, 0.000000000000000000, 1.000000000000000000 ) ) ;
#4011 = ORIENTED_EDGE ( 'NONE', *, *, #12622, .F. ) ;
#4012 = SURFACE_SIDE_STYLE ('',( #11028 ) ) ;
#4013 = DIRECTION ( 'NONE',  ( 0.8746197071345590546, -0.4848096202550628009, 0.000000000000000000 ) ) ;
#4014 = ADVANCED_FACE ( 'NONE', ( #32 ), #6717, .T. ) ;
#4015 = CYLINDRICAL_SURFACE ( 'NONE', #6555, 0.7892041907098262810 ) ;
#4016 = AXIS2_PLACEMENT_3D ( 'NONE', #14085, #8242, #7082 ) ;
#4017 = CARTESIAN_POINT ( 'NONE',  ( 20.86173033120691045, -57.24929059928630437, 0.000000000000000000 ) ) ;
#4018 = CARTESIAN_POINT ( 'NONE',  ( -3.999999999999976019, -72.24929059928631148, -32.99999999999998579 ) ) ;
#4019 = FACE_OUTER_BOUND ( 'NONE', #7636, .T. ) ;
#4020 = CARTESIAN_POINT ( 'NONE',  ( -25.46282903980763024, -6.565599745187293834, -48.00000000000012079 ) ) ;
#4021 = EDGE_CURVE ( 'NONE', #6859, #5990, #7026, .T. ) ;
#4022 = ORIENTED_EDGE ( 'NONE', *, *, #7061, .T. ) ;
#4023 = CARTESIAN_POINT ( 'NONE',  ( 35.09024216261268236, -47.02718879221286841, -2.731995254387835192 ) ) ;
#4024 = ORIENTED_EDGE ( 'NONE', *, *, #11631, .T. ) ;
#4025 = CARTESIAN_POINT ( 'NONE',  ( -1.197457146693683194, -2.220571218158922999, -57.50000000000012079 ) ) ;
#4026 = CYLINDRICAL_SURFACE ( 'NONE', #308, 4.276034690655509785 ) ;
#4027 = VERTEX_POINT ( 'NONE', #7959 ) ;
#4028 = DIRECTION ( 'NONE',  ( 0.000000000000000000, 0.000000000000000000, 1.000000000000000000 ) ) ;
#4029 = CYLINDRICAL_SURFACE ( 'NONE', #4832, 0.5000000000000002220 ) ;
#4030 = CARTESIAN_POINT ( 'NONE',  ( 48.00000000000000000, -2.249290599286307479, 33.00000000000012790 ) ) ;
#4031 = EDGE_CURVE ( 'NONE', #246, #1863, #1018, .T. ) ;
#4032 = DIRECTION ( 'NONE',  ( 0.8208219420614786266, -0.4549890321264269955, -0.3453061251629919726 ) ) ;
#4033 = ADVANCED_FACE ( 'NONE', ( #6789 ), #11479, .F. ) ;
#4034 = EDGE_CURVE ( 'NONE', #8031, #9462, #9263, .T. ) ;
#4035 = EDGE_CURVE ( 'NONE', #14995, #3495, #8870, .T. ) ;
#4036 = DIRECTION ( 'NONE',  ( 0.000000000000000000, 0.000000000000000000, -1.000000000000000000 ) ) ;
#4037 = DIRECTION ( 'NONE',  ( 0.000000000000000000, 1.000000000000000000, 2.312964634635740689E-15 ) ) ;
#4038 = VERTEX_POINT ( 'NONE', #15035 ) ;
#4039 = CARTESIAN_POINT ( 'NONE',  ( 96.29968967959054282, 25.52935533987996664, 84.20452624982236500 ) ) ;
#4040 = EDGE_LOOP ( 'NONE', ( #7922, #13761, #4377, #4768 ) ) ;
#4041 = EDGE_CURVE ( 'NONE', #6176, #9708, #1990, .T. ) ;
#4042 = CARTESIAN_POINT ( 'NONE',  ( -24.54250511040913096, 2.674312581063694516, 47.50000000000008527 ) ) ;
#4043 = VERTEX_POINT ( 'NONE', #15113 ) ;
#4044 = CYLINDRICAL_SURFACE ( 'NONE', #3197, 10.00000000000000178 ) ;
#4045 = CARTESIAN_POINT ( 'NONE',  ( 69.41635813202618976, -3.305880236131207184, 71.46816610982854456 ) ) ;
#4046 = ORIENTED_EDGE ( 'NONE', *, *, #4183, .T. ) ;
#4047 = FACE_OUTER_BOUND ( 'NONE', #5621, .T. ) ;
#4048 = CARTESIAN_POINT ( 'NONE',  ( 58.44010239582257071, -7.290881550929530164, 62.84860122826521689 ) ) ;
#4049 = VERTEX_POINT ( 'NONE', #1731 ) ;
#4050 = CARTESIAN_POINT ( 'NONE',  ( 29.87892709566675009, -63.30956378474007806, -2.875213255995181960 ) ) ;
#4051 = VERTEX_POINT ( 'NONE', #6571 ) ;
#4052 = EDGE_CURVE ( 'NONE', #8396, #12161, #13505, .T. ) ;
#4053 = DIRECTION ( 'NONE',  ( -0.8746197071345569451, 0.4848096202550666312, 0.000000000000000000 ) ) ;
#4054 = DIRECTION ( 'NONE',  ( 1.000000000000000000, 0.000000000000000000, 0.000000000000000000 ) ) ;
#4055 = LINE ( 'NONE', #13452, #8558 ) ;
#4056 = CYLINDRICAL_SURFACE ( 'NONE', #9926, 0.5000000000000001110 ) ;
#4057 = ORIENTED_EDGE ( 'NONE', *, *, #8623, .T. ) ;
#4058 = CIRCLE ( 'NONE', #2364, 4.194885682587998765 ) ;
#4059 = DIRECTION ( 'NONE',  ( 0.000000000000000000, 1.000000000000000000, -0.000000000000000000 ) ) ;
#4060 = EDGE_CURVE ( 'NONE', #10618, #1834, #9970, .T. ) ;
#4061 = ORIENTED_EDGE ( 'NONE', *, *, #9606, .F. ) ;
#4062 = ORIENTED_EDGE ( 'NONE', *, *, #14035, .F. ) ;
#4063 = CARTESIAN_POINT ( 'NONE',  ( 104.0000000000000426, 15.25070940071369563, 33.00000000000012790 ) ) ;
#4064 = PRODUCT_CONTEXT ( 'NONE', #8716, 'mechanical' ) ;
#4065 = CARTESIAN_POINT ( 'NONE',  ( 58.00000000000000711, -2.249290599286309256, 71.19766410831374515 ) ) ;
#4066 = FACE_OUTER_BOUND ( 'NONE', #7365, .T. ) ;
#4067 = CIRCLE ( 'NONE', #10976, 9.500000000000001776 ) ;
#4068 = ORIENTED_EDGE ( 'NONE', *, *, #7117, .F. ) ;
#4069 = PLANE ( 'NONE',  #13471 ) ;
#4070 = FACE_OUTER_BOUND ( 'NONE', #8352, .T. ) ;
#4071 = DIRECTION ( 'NONE',  ( -0.000000000000000000, 0.000000000000000000, 1.000000000000000000 ) ) ;
#4072 = CARTESIAN_POINT ( 'NONE',  ( 11.13001753994803344, -62.42480215138046873, -2.585081138721826211 ) ) ;
#4073 = EDGE_LOOP ( 'NONE', ( #1869, #5284, #5139, #13523 ) ) ;
#4074 = DIRECTION ( 'NONE',  ( -1.000000000000000000, 0.000000000000000000, 0.000000000000000000 ) ) ;
#4075 = ADVANCED_FACE ( 'NONE', ( #6648 ), #14654, .T. ) ;
#4076 = EDGE_CURVE ( 'NONE', #13835, #7432, #7802, .T. ) ;
#4077 = AXIS2_PLACEMENT_3D ( 'NONE', #9848, #13373, #9987 ) ;
#4078 = CARTESIAN_POINT ( 'NONE',  ( -9.148597373295839219, 2.167486929505451076, 48.18452149279841024 ) ) ;
#4079 = EDGE_LOOP ( 'NONE', ( #9449, #4802, #6054, #101 ) ) ;
#4080 = FILL_AREA_STYLE_COLOUR ( '', #14068 ) ;
#4081 = CARTESIAN_POINT ( 'NONE',  ( 33.25707175992479847, -58.63671300496867644, -1.826958383926200247 ) ) ;
#4082 = CARTESIAN_POINT ( 'NONE',  ( 0.000000000000000000, 0.000000000000000000, 0.000000000000000000 ) ) ;
#4083 = DIRECTION ( 'NONE',  ( -0.000000000000000000, -0.000000000000000000, 1.000000000000000000 ) ) ;
#4084 = VERTEX_POINT ( 'NONE', #9122 ) ;
#4085 = VECTOR ( 'NONE', #3753, 1000.000000000000000 ) ;
#4086 = CIRCLE ( 'NONE', #14915, 3.999999999999996003 ) ;
#4087 = VECTOR ( 'NONE', #9353, 1000.000000000000000 ) ;
#4088 = CARTESIAN_POINT ( 'NONE',  ( -16.99999999999998579, -2.249290599286303927, -38.00000000000012079 ) ) ;
#4089 = CARTESIAN_POINT ( 'NONE',  ( -5.290523468902621929, 4.522075770548486418, -48.00000000000012079 ) ) ;
#4090 =( BOUNDED_SURFACE ( )  B_SPLINE_SURFACE ( 3, 2, ( 
 ( #2162, #11540, #998 ),
 ( #10406, #14156, #8534 ),
 ( #7225, #12069, #1373 ),
 ( #228, #8316, #9771 ) ),
 .UNSPECIFIED., .F., .F., .F. ) 
 B_SPLINE_SURFACE_WITH_KNOTS ( ( 4, 4 ),
 ( 3, 3 ),
 ( -3.469446951953614189E-18, 0.006683255761480919911 ),
 ( 0.000000000000000000, 1.000000000000000000 ),
 .UNSPECIFIED. ) 
 GEOMETRIC_REPRESENTATION_ITEM ( )  RATIONAL_B_SPLINE_SURFACE ( (
 ( 1.000000000000000000, 0.7071067811865500152, 1.000000000000000000),
 ( 1.000000000000000000, 0.7035788727800782461, 1.000000000000000000),
 ( 1.000000000000000000, 0.6996284196041381298, 1.000000000000000000),
 ( 1.000000000000000000, 0.6947298545087535748, 1.000000000000000000) ) ) 
 REPRESENTATION_ITEM ( '' )  SURFACE ( )  );
#4091 = FACE_OUTER_BOUND ( 'NONE', #8052, .T. ) ;
#4092 = EDGE_CURVE ( 'NONE', #2180, #2895, #7170, .T. ) ;
#4093 = ADVANCED_FACE ( 'NONE', ( #4260 ), #10496, .T. ) ;
#4094 = CIRCLE ( 'NONE', #8047, 3.999999999999999112 ) ;
#4095 =( GEOMETRIC_REPRESENTATION_CONTEXT ( 3 ) GLOBAL_UNCERTAINTY_ASSIGNED_CONTEXT ( ( #4895 ) ) GLOBAL_UNIT_ASSIGNED_CONTEXT ( ( #14256, #21, #11545 ) ) REPRESENTATION_CONTEXT ( 'NONE', 'WORKASPACE' ) );
#4096 = VERTEX_POINT ( 'NONE', #7119 ) ;
#4097 = MANIFOLD_SOLID_BREP ( 'Move Face2', #11190 ) ;
#4098 = CARTESIAN_POINT ( 'NONE',  ( 28.99843454536937415, -51.89470720436212048, -4.215327499024904334 ) ) ;
#4099 = VECTOR ( 'NONE', #8005, 1000.000000000000000 ) ;
#4100 = ORIENTED_EDGE ( 'NONE', *, *, #7567, .T. ) ;
#4101 = CARTESIAN_POINT ( 'NONE',  ( -25.21252699837112132, -6.998437922861944216, 48.36782213136056896 ) ) ;
#4102 = CARTESIAN_POINT ( 'NONE',  ( -26.99999999999998224, -69.24929059928631148, 33.00000000000000711 ) ) ;
#4103 = TOROIDAL_SURFACE ( 'NONE', #10019, 1.000000000000000000, 0.5000000000000000000 ) ;
#4104 = ORIENTED_EDGE ( 'NONE', *, *, #7251, .T. ) ;
#4105 = FACE_BOUND ( 'NONE', #10933, .T. ) ;
#4106 = FACE_OUTER_BOUND ( 'NONE', #5346, .T. ) ;
#4107 = ORIENTED_EDGE ( 'NONE', *, *, #3785, .F. ) ;
#4108 = DIRECTION ( 'NONE',  ( -0.8746197071345569451, 0.4848096202550666312, 0.000000000000000000 ) ) ;
#4109 = AXIS2_PLACEMENT_3D ( 'NONE', #724, #2200, #10131 ) ;
#4110 = CYLINDRICAL_SURFACE ( 'NONE', #8317, 2.499999999999995115 ) ;
#4111 = CIRCLE ( 'NONE', #6109, 3.694885682588112896 ) ;
#4112 = VECTOR ( 'NONE', #10512, 1000.000000000000000 ) ;
#4113 = VECTOR ( 'NONE', #7000, 1000.000000000000000 ) ;
#4114 = DIRECTION ( 'NONE',  ( 0.000000000000000000, -0.000000000000000000, -1.000000000000000000 ) ) ;
#4115 = CARTESIAN_POINT ( 'NONE',  ( -8.787473001628837821, 2.499856724289235554, -57.50000000000012079 ) ) ;
#4116 = ORIENTED_EDGE ( 'NONE', *, *, #6408, .F. ) ;
#4117 = ORIENTED_EDGE ( 'NONE', *, *, #11909, .T. ) ;
#4118 = CARTESIAN_POINT ( 'NONE',  ( 9.657637030002515388, -61.15506547911440549, 2.039555069691858513 ) ) ;
#4119 = EDGE_CURVE ( 'NONE', #4131, #14644, #7901, .T. ) ;
#4120 = EDGE_LOOP ( 'NONE', ( #11613, #3500, #4062, #1230 ) ) ;
#4121 = CARTESIAN_POINT ( 'NONE',  ( 20.86173033120691045, -57.24929059928630437, 0.000000000000000000 ) ) ;
#4122 = AXIS2_PLACEMENT_3D ( 'NONE', #12400, #4074, #3163 ) ;
#4123 = ORIENTED_EDGE ( 'NONE', *, *, #5084, .T. ) ;
#4124 = DIRECTION ( 'NONE',  ( 0.8208219420614786266, -0.4549890321264268844, -0.3453061251629920281 ) ) ;
#4125 = DIRECTION ( 'NONE',  ( 0.8746197071345569451, -0.4848096202550666312, 0.000000000000000000 ) ) ;
#4126 = VECTOR ( 'NONE', #11890, 1000.000000000000000 ) ;
#4127 = DIRECTION ( 'NONE',  ( 0.5006040828730228265, -0.8656763553493070917, 0.000000000000000000 ) ) ;
#4128 = CARTESIAN_POINT ( 'NONE',  ( -21.85476584171713199, 5.329050157244540564, -57.50000000000012079 ) ) ;
#4129 = ORIENTED_EDGE ( 'NONE', *, *, #10653, .T. ) ;
#4130 = LINE ( 'NONE', #3984, #7179 ) ;
#4131 = VERTEX_POINT ( 'NONE', #4500 ) ;
#4132 = EDGE_CURVE ( 'NONE', #8533, #3352, #3478, .T. ) ;
#4133 = EDGE_CURVE ( 'NONE', #6293, #10292, #11323, .T. ) ;
#4134 = CYLINDRICAL_SURFACE ( 'NONE', #7640, 3.951771890309584645 ) ;
#4135 = DIRECTION ( 'NONE',  ( 0.000000000000000000, 0.000000000000000000, 1.000000000000000000 ) ) ;
#4136 = CARTESIAN_POINT ( 'NONE',  ( -9.271822474830681671, -6.861803161813159413, 48.00000000000019895 ) ) ;
#4137 = EDGE_LOOP ( 'NONE', ( #3075, #12175, #3600, #10609 ) ) ;
#4138 = CARTESIAN_POINT ( 'NONE',  ( -21.66581936427349575, -2.249290599286304371, -50.50000000000012079 ) ) ;
#4139 = ORIENTED_EDGE ( 'NONE', *, *, #14960, .F. ) ;
#4140 = ORIENTED_EDGE ( 'NONE', *, *, #1789, .T. ) ;
#4141 = ORIENTED_EDGE ( 'NONE', *, *, #4763, .T. ) ;
#4142 = EDGE_CURVE ( 'NONE', #14923, #5424, #5818, .T. ) ;
#4143 = SURFACE_SIDE_STYLE ('',( #7850 ) ) ;
#4144 = ADVANCED_FACE ( 'NONE', ( #11572 ), #13072, .T. ) ;
#4145 = CARTESIAN_POINT ( 'NONE',  ( -16.99999999999998579, -2.249290599286303927, 57.50000000000012079 ) ) ;
#4146 = CARTESIAN_POINT ( 'NONE',  ( -25.46282903980766932, -6.565599745187317815, -58.00000000000012079 ) ) ;
#4147 = VECTOR ( 'NONE', #10490, 1000.000000000000000 ) ;
#4148 = CIRCLE ( 'NONE', #2692, 0.4999999999999995559 ) ;
#4149 = CARTESIAN_POINT ( 'NONE',  ( -3.285520523750506516, 5.681530634152946568, 48.50000000000012079 ) ) ;
#4150 = EDGE_LOOP ( 'NONE', ( #5908, #10607, #13297, #279 ) ) ;
#4151 = CARTESIAN_POINT ( 'NONE',  ( -8.590985667557523797, 2.187759657648595368, -48.00000000000012079 ) ) ;
#4152 = CARTESIAN_POINT ( 'NONE',  ( 64.96908986428803701, -11.35320032814772517, 71.45158253113490332 ) ) ;
#4153 = CARTESIAN_POINT ( 'NONE',  ( 33.62991918736606323, -56.17545244456535158, -1.862977194132048764 ) ) ;
#4154 = DIRECTION ( 'NONE',  ( 1.000000000000000000, 0.000000000000000000, 0.000000000000000000 ) ) ;
#4155 = CARTESIAN_POINT ( 'NONE',  ( 11.84453356674737101, -63.30956378474044044, -2.875213255991756700 ) ) ;
#4156 = VERTEX_POINT ( 'NONE', #43 ) ;
#4157 = CARTESIAN_POINT ( 'NONE',  ( 33.62061467546807592, -56.17744385466402690, 1.865378520189665545 ) ) ;
#4158 = VECTOR ( 'NONE', #3016, 1000.000000000000000 ) ;
#4159 = CONICAL_SURFACE ( 'NONE', #13037, 2.524999999999999467, 0.7853981633973787790 ) ;
#4160 = CARTESIAN_POINT ( 'NONE',  ( -12.99999999999998757, -2.249290599286301706, 33.00000000000009948 ) ) ;
#4161 = ORIENTED_EDGE ( 'NONE', *, *, #10247, .F. ) ;
#4162 = CARTESIAN_POINT ( 'NONE',  ( 27.41707935315583455, -67.70775585802556407, -4.528449950254390899 ) ) ;
#4163 = CARTESIAN_POINT ( 'NONE',  ( -24.54316048551696383, -7.158540021523408292, -48.37147253714708484 ) ) ;
#4164 = ORIENTED_EDGE ( 'NONE', *, *, #6398, .T. ) ;
#4165 = CARTESIAN_POINT ( 'NONE',  ( -28.95977857253364007, -8.587818791446682809, -58.00000000000012079 ) ) ;
#4166 = EDGE_CURVE ( 'NONE', #13981, #13835, #5800, .T. ) ;
#4167 = TOROIDAL_SURFACE ( 'NONE', #12296, 8.500000000000000000, 0.5000000000000000000 ) ;
#4168 = EDGE_CURVE ( 'NONE', #3262, #341, #951, .T. ) ;
#4169 = CARTESIAN_POINT ( 'NONE',  ( 88.00000000000000000, 23.25070940071369208, 84.20452624982236500 ) ) ;
#4170 = DIRECTION ( 'NONE',  ( 0.000000000000000000, 0.000000000000000000, 1.000000000000000000 ) ) ;
#4171 = CARTESIAN_POINT ( 'NONE',  ( 68.00000000000001421, 1.887379141862766624E-13, 139.1143251403882459 ) ) ;
#4172 = VERTEX_POINT ( 'NONE', #15048 ) ;
#4173 = LINE ( 'NONE', #8874, #3187 ) ;
#4174 = ORIENTED_EDGE ( 'NONE', *, *, #10349, .F. ) ;
#4175 = FACE_BOUND ( 'NONE', #1609, .T. ) ;
#4176 = DIRECTION ( 'NONE',  ( -0.000000000000000000, 0.000000000000000000, 1.000000000000000000 ) ) ;
#4177 = AXIS2_PLACEMENT_3D ( 'NONE', #4589, #14638, #6716 ) ;
#4178 = ORIENTED_EDGE ( 'NONE', *, *, #2571, .F. ) ;
#4179 = CARTESIAN_POINT ( 'NONE',  ( -8.958610760419841057, 1.823307968896474840, 58.00000000000012079 ) ) ;
#4180 = CARTESIAN_POINT ( 'NONE',  ( 13.86173033120691578, -69.39711819508849544, -3.710481764567795437 ) ) ;
#4181 = EDGE_CURVE ( 'NONE', #4272, #13804, #6672, .T. ) ;
#4182 = CARTESIAN_POINT ( 'NONE',  ( 11.13001753994774212, -62.42480215138011346, 2.585081138721638361 ) ) ;
#4183 = EDGE_CURVE ( 'NONE', #6287, #12282, #13553, .T. ) ;
#4184 = CARTESIAN_POINT ( 'NONE',  ( 10.43256186016586184, -53.71411213207043289, 3.559347964322298719 ) ) ;
#4185 = FACE_OUTER_BOUND ( 'NONE', #7947, .T. ) ;
#4186 = CARTESIAN_POINT ( 'NONE',  ( -12.14523415828296216, -9.827631355817223024, -48.50000000000012079 ) ) ;
#4187 = LINE ( 'NONE', #7743, #7075 ) ;
#4188 = ORIENTED_EDGE ( 'NONE', *, *, #12428, .F. ) ;
#4189 = PLANE ( 'NONE',  #8535 ) ;
#4190 = AXIS2_PLACEMENT_3D ( 'NONE', #10593, #7205, #8449 ) ;
#4191 = ORIENTED_EDGE ( 'NONE', *, *, #5015, .F. ) ;
#4192 = CARTESIAN_POINT ( 'NONE',  ( 63.04142083571589694, -2.691337429055927988, 48.51982618741349285 ) ) ;
#4193 = VECTOR ( 'NONE', #1182, 1000.000000000000000 ) ;
#4194 = ORIENTED_EDGE ( 'NONE', *, *, #12608, .T. ) ;
#4195 = CARTESIAN_POINT ( 'NONE',  ( -29.99999999999998224, -69.24929059928631148, 33.00000000000000000 ) ) ;
#4196 = VECTOR ( 'NONE', #2694, 1000.000000000000000 ) ;
#4197 = CARTESIAN_POINT ( 'NONE',  ( 55.86211336638498182, 2.337731330496643167, 60.61639468829817190 ) ) ;
#4198 = EDGE_CURVE ( 'NONE', #8129, #14139, #5750, .T. ) ;
#4199 = CARTESIAN_POINT ( 'NONE',  ( 50.07597535787931520, -2.249290599286308368, 39.50000000000012790 ) ) ;
#4200 = LINE ( 'NONE', #4128, #10170 ) ;
#4201 = ORIENTED_EDGE ( 'NONE', *, *, #1326, .F. ) ;
#4202 = CARTESIAN_POINT ( 'NONE',  ( 27.86203511185233594, -69.48056866272028742, -4.214447830835834630 ) ) ;
#4203 = AXIS2_PLACEMENT_3D ( 'NONE', #6960, #12969, #7112 ) ;
#4204 = ORIENTED_EDGE ( 'NONE', *, *, #10943, .F. ) ;
#4205 = AXIS2_PLACEMENT_3D ( 'NONE', #13603, #2057, #7756 ) ;
#4206 = AXIS2_PLACEMENT_3D ( 'NONE', #6205, #12116, #5181 ) ;
#4207 = CARTESIAN_POINT ( 'NONE',  ( -28.70947653109703168, -9.020656969121420232, -57.50000000000012079 ) ) ;
#4208 = CARTESIAN_POINT ( 'NONE',  ( 11.41872426162122345, -52.33170319195679099, -3.962365649671490075 ) ) ;
#4209 = LINE ( 'NONE', #4367, #2293 ) ;
#4210 = CARTESIAN_POINT ( 'NONE',  ( 25.81270058232203013, 0.000000000000000000, -33.00000000000012790 ) ) ;
#4211 = ORIENTED_EDGE ( 'NONE', *, *, #8572, .F. ) ;
#4212 = CARTESIAN_POINT ( 'NONE',  ( -65.00000000000001421, -87.24929059928631148, -19.99999999999999645 ) ) ;
#4213 = ORIENTED_EDGE ( 'NONE', *, *, #6762, .F. ) ;
#4214 = ORIENTED_EDGE ( 'NONE', *, *, #4031, .F. ) ;
#4215 = AXIS2_PLACEMENT_3D ( 'NONE', #14941, #13785, #11171 ) ;
#4216 = ORIENTED_EDGE ( 'NONE', *, *, #9100, .T. ) ;
#4217 = CIRCLE ( 'NONE', #1030, 6.484807146443463566 ) ;
#4218 = ADVANCED_FACE ( 'NONE', ( #12903 ), #12030, .F. ) ;
#4219 = AXIS2_PLACEMENT_3D ( 'NONE', #6391, #14549, #6467 ) ;
#4220 = CONTEXT_DEPENDENT_SHAPE_REPRESENTATION ( #2805, #401 ) ;
#4221 = DIRECTION ( 'NONE',  ( 0.000000000000000000, 0.000000000000000000, 1.000000000000000000 ) ) ;
#4222 = CARTESIAN_POINT ( 'NONE',  ( 82.49066175147797253, 23.25070940071369208, 33.00000000000012790 ) ) ;
#4223 = DIRECTION ( 'NONE',  ( 9.251858538542971581E-17, 1.000000000000000000, 0.000000000000000000 ) ) ;
#4224 = ORIENTED_EDGE ( 'NONE', *, *, #8363, .T. ) ;
#4225 = CARTESIAN_POINT ( 'NONE',  ( 58.00000000000000711, -2.249290599286309256, 48.51982618741349285 ) ) ;
#4226 = VECTOR ( 'NONE', #6256, 1000.000000000000000 ) ;
#4227 = LINE ( 'NONE', #6617, #13746 ) ;
#4228 = EDGE_CURVE ( 'NONE', #13012, #8978, #11889, .T. ) ;
#4229 = CARTESIAN_POINT ( 'NONE',  ( 16.53849081582479386, -69.39711819508849544, 5.637959728397555992 ) ) ;
#4230 = CARTESIAN_POINT ( 'NONE',  ( 12.48247979829434584, -64.27177309650687675, -3.135762038895900439 ) ) ;
#4231 = AXIS2_PLACEMENT_3D ( 'NONE', #3009, #6531, #6611 ) ;
#4232 = EDGE_CURVE ( 'NONE', #9462, #5523, #2654, .T. ) ;
#4233 = EDGE_LOOP ( 'NONE', ( #4788, #12929, #10018, #8945 ) ) ;
#4234 = CARTESIAN_POINT ( 'NONE',  ( 69.46221311397140141, -2.886128745360726278, 73.10613156102081689 ) ) ;
#4235 = AXIS2_PLACEMENT_3D ( 'NONE', #3444, #10978, #13215 ) ;
#4236 = LINE ( 'NONE', #4394, #3699 ) ;
#4237 = VERTEX_POINT ( 'NONE', #7343 ) ;
#4238 = CARTESIAN_POINT ( 'NONE',  ( 28.09009917991004812, -65.27414832489905905, -4.302972696997105828 ) ) ;
#4239 = FACE_OUTER_BOUND ( 'NONE', #7810, .T. ) ;
#4240 = EDGE_CURVE ( 'NONE', #3262, #3110, #9743, .T. ) ;
#4241 = DIRECTION ( 'NONE',  ( 0.000000000000000000, 1.000000000000000000, 0.000000000000000000 ) ) ;
#4242 = FACE_OUTER_BOUND ( 'NONE', #10497, .T. ) ;
#4243 = ORIENTED_EDGE ( 'NONE', *, *, #4577, .F. ) ;
#4244 = PRODUCT_DEFINITION_SHAPE ( 'NONE', 'NONE',  #1199 ) ;
#4245 = DIRECTION ( 'NONE',  ( -0.000000000000000000, 1.734723475976817547E-15, 1.000000000000000000 ) ) ;
#4246 = AXIS2_PLACEMENT_3D ( 'NONE', #2997, #7535, #459 ) ;
#4247 = CARTESIAN_POINT ( 'NONE',  ( 29.69047892279256118, -53.28399145779480506, 4.141535524925028966 ) ) ;
#4248 = CARTESIAN_POINT ( 'NONE',  ( -25.15752072101212278, 2.619472661158555038, -48.00000000000012079 ) ) ;
#4249 = CARTESIAN_POINT ( 'NONE',  ( -25.34903703195771385, -6.790201970332132575, -48.06291368403887532 ) ) ;
#4250 = VERTEX_POINT ( 'NONE', #6048 ) ;
#4251 = AXIS2_PLACEMENT_3D ( 'NONE', #15205, #11579, #15130 ) ;
#4252 = CARTESIAN_POINT ( 'NONE',  ( 31.88156390563087683, -61.30062302791112927, 2.840369378987805060 ) ) ;
#4253 = EDGE_CURVE ( 'NONE', #3440, #15191, #1032, .T. ) ;
#4254 = ORIENTED_EDGE ( 'NONE', *, *, #12710, .F. ) ;
#4255 = CARTESIAN_POINT ( 'NONE',  ( 23.10474973039556801, -52.24929059928630437, -5.564967562786270250 ) ) ;
#4256 = DIRECTION ( 'NONE',  ( 0.9744556954135528137, 0.2245798247307385087, -0.000000000000000000 ) ) ;
#4257 = EDGE_LOOP ( 'NONE', ( #5302, #13233, #12869, #496, #1818 ) ) ;
#4258 = DIRECTION ( 'NONE',  ( 0.000000000000000000, 0.000000000000000000, 1.000000000000000000 ) ) ;
#4259 = CARTESIAN_POINT ( 'NONE',  ( -2.016677571526633510E-15, 23.25070940071368497, 33.00000000000012790 ) ) ;
#4260 = FACE_OUTER_BOUND ( 'NONE', #9077, .T. ) ;
#4261 = CARTESIAN_POINT ( 'NONE',  ( 10.27153280171312666, -52.79510901551753221, 2.616251790959217782 ) ) ;
#4262 = DIRECTION ( 'NONE',  ( 0.000000000000000000, 0.000000000000000000, 1.000000000000000000 ) ) ;
#4263 = DIRECTION ( 'NONE',  ( -0.000000000000000000, -0.000000000000000000, -1.000000000000000000 ) ) ;
#4264 = CARTESIAN_POINT ( 'NONE',  ( 65.00000000000001421, -85.27429059928628874, -19.99999999999999645 ) ) ;
#4265 = DIRECTION ( 'NONE',  ( -0.9421718071228325497, -3.620235254251614364E-16, -0.3351302520855077294 ) ) ;
#4266 = ORIENTED_EDGE ( 'NONE', *, *, #13085, .F. ) ;
#4267 = CARTESIAN_POINT ( 'NONE',  ( 8.597635011448852893, -59.20619211347771227, 2.502190571104538463 ) ) ;
#4268 = EDGE_CURVE ( 'NONE', #5864, #9470, #1497, .T. ) ;
#4269 = ADVANCED_FACE ( 'NONE', ( #411 ), #6125, .F. ) ;
#4270 = ORIENTED_EDGE ( 'NONE', *, *, #4521, .T. ) ;
#4271 = CARTESIAN_POINT ( 'NONE',  ( 31.88917822179636374, -54.14192065903539230, -3.328125142887244703 ) ) ;
#4272 = VERTEX_POINT ( 'NONE', #1575 ) ;
#4273 = DIRECTION ( 'NONE',  ( -0.5394184268574488961, 0.8420378618367674317, 0.000000000000000000 ) ) ;
#4274 = LINE ( 'NONE', #10061, #13669 ) ;
#4275 = CARTESIAN_POINT ( 'NONE',  ( -8.537170960192327129, 2.067018546614582508, -57.50000000000012079 ) ) ;
#4276 = CARTESIAN_POINT ( 'NONE',  ( 53.81626139532630759, -85.24929059928631148, 11.78977872328355048 ) ) ;
#4277 = ORIENTED_EDGE ( 'NONE', *, *, #12708, .F. ) ;
#4278 = PLANE ( 'NONE',  #4454 ) ;
#4279 = ORIENTED_EDGE ( 'NONE', *, *, #6928, .F. ) ;
#4280 = DIRECTION ( 'NONE',  ( 0.000000000000000000, 0.000000000000000000, 1.000000000000000000 ) ) ;
#4281 = CARTESIAN_POINT ( 'NONE',  ( 8.090330977888115171, -56.40460476644708621, -2.550424528238877553 ) ) ;
#4282 = DIRECTION ( 'NONE',  ( -0.7546336727145983581, 0.5961293309129265250, 0.2741493039031521195 ) ) ;
#4283 = DIRECTION ( 'NONE',  ( 8.673617379884035472E-17, -1.000000000000000000, 0.000000000000000000 ) ) ;
#4284 = ORIENTED_EDGE ( 'NONE', *, *, #8437, .T. ) ;
#4285 = VERTEX_POINT ( 'NONE', #10892 ) ;
#4286 = EDGE_CURVE ( 'NONE', #4371, #3688, #5113, .T. ) ;
#4287 = EDGE_CURVE ( 'NONE', #8779, #1998, #3929, .T. ) ;
#4288 = CYLINDRICAL_SURFACE ( 'NONE', #1904, 4.000000000000000000 ) ;
#4289 = ORIENTED_EDGE ( 'NONE', *, *, #881, .F. ) ;
#4290 = LINE ( 'NONE', #980, #7928 ) ;
#4291 = ORIENTED_EDGE ( 'NONE', *, *, #230, .F. ) ;
#4292 = ORIENTED_EDGE ( 'NONE', *, *, #14114, .T. ) ;
#4293 = DIRECTION ( 'NONE',  ( 0.000000000000000000, 0.000000000000000000, 1.000000000000000000 ) ) ;
#4294 = DIRECTION ( 'NONE',  ( -0.000000000000000000, -0.000000000000000000, 1.000000000000000000 ) ) ;
#4295 = CARTESIAN_POINT ( 'NONE',  ( 68.90181265608016759, -8.292264031936127822, 72.19766410831374515 ) ) ;
#4296 = CARTESIAN_POINT ( 'NONE',  ( 0.000000000000000000, 29.52935533987996664, 0.000000000000000000 ) ) ;
#4297 = CARTESIAN_POINT ( 'NONE',  ( -28.70947653109703168, -9.020656969121420232, -48.50000000000012079 ) ) ;
#4298 = ORIENTED_EDGE ( 'NONE', *, *, #5504, .T. ) ;
#4299 = CARTESIAN_POINT ( 'NONE',  ( 65.05854647941774260, -11.28415211138448981, 71.39260873926113504 ) ) ;
#4300 = CARTESIAN_POINT ( 'NONE',  ( 33.63314816004646701, -56.83321641073668218, -1.823854045754459641 ) ) ;
#4301 = LINE ( 'NONE', #13708, #6229 ) ;
#4302 = CARTESIAN_POINT ( 'NONE',  ( 13.41074896738031264, -66.37912134691028143, -3.509717431437874069 ) ) ;
#4303 = ORIENTED_EDGE ( 'NONE', *, *, #3343, .F. ) ;
#4304 = DIRECTION ( 'NONE',  ( 0.9816271834495682302, 0.1908089953667485572, 0.000000000000000000 ) ) ;
#4305 = B_SPLINE_CURVE_WITH_KNOTS ( 'NONE', 3,
 ( #624, #5329, #13339, #13268 ),
 .UNSPECIFIED., .F., .F.,
 ( 4, 4 ),
 ( 0.000000000000000000, 0.001771361151111836745 ),
 .UNSPECIFIED. ) ;
#4306 = CARTESIAN_POINT ( 'NONE',  ( 63.43853564383336874, -3.373351419973840581, 48.51982618741349285 ) ) ;
#4307 = ADVANCED_FACE ( 'NONE', ( #6344 ), #2500, .F. ) ;
#4308 = ORIENTED_EDGE ( 'NONE', *, *, #1792, .F. ) ;
#4309 =( NAMED_UNIT ( * ) PLANE_ANGLE_UNIT ( ) SI_UNIT ( $, .RADIAN. ) );
#4310 = FACE_OUTER_BOUND ( 'NONE', #3893, .T. ) ;
#4311 = AXIS2_PLACEMENT_3D ( 'NONE', #4296, #4456, #8001 ) ;
#4312 = CARTESIAN_POINT ( 'NONE',  ( -5.040221427466109461, 4.089237592873834259, -48.00000000000012079 ) ) ;
#4313 = CARTESIAN_POINT ( 'NONE',  ( 65.00000000000001421, -85.27429059928628874, -17.49999999999999645 ) ) ;
#4314 = ORIENTED_EDGE ( 'NONE', *, *, #7498, .T. ) ;
#4315 = EDGE_CURVE ( 'NONE', #1125, #12049, #8436, .T. ) ;
#4316 = DIRECTION ( 'NONE',  ( 0.000000000000000000, 0.000000000000000000, -1.000000000000000000 ) ) ;
#4317 = ADVANCED_FACE ( 'NONE', ( #272 ), #11955, .F. ) ;
#4318 = CARTESIAN_POINT ( 'NONE',  ( 71.64423341085262109, -14.38582895075279211, 72.19766410831374515 ) ) ;
#4319 = CARTESIAN_POINT ( 'NONE',  ( 12.06345512429583344, -63.57773214734891098, 2.964070158660694787 ) ) ;
#4320 = CARTESIAN_POINT ( 'NONE',  ( 40.33162949095117966, 23.25070940071368852, 33.00000000000012790 ) ) ;
#4321 = EDGE_CURVE ( 'NONE', #3040, #965, #3801, .T. ) ;
#4322 = CARTESIAN_POINT ( 'NONE',  ( -25.01741698508091005, -6.338425579613558014, -48.00000000000010658 ) ) ;
#4323 = EDGE_CURVE ( 'NONE', #14286, #1582, #10620, .T. ) ;
#4324 = CIRCLE ( 'NONE', #9499, 3.999999999999994227 ) ;
#4325 = EDGE_LOOP ( 'NONE', ( #13818, #7388, #6167, #10076 ) ) ;
#4326 = CARTESIAN_POINT ( 'NONE',  ( 42.07846078193830408, 23.25070940071368852, 33.00000000000012790 ) ) ;
#4327 = ORIENTED_EDGE ( 'NONE', *, *, #13432, .T. ) ;
#4328 = DIRECTION ( 'NONE',  ( 0.000000000000000000, 1.000000000000000000, 0.000000000000000000 ) ) ;
#4329 = CARTESIAN_POINT ( 'NONE',  ( 130.4454129427046496, 23.25070940071369563, 13.14990448602692474 ) ) ;
#4330 = EDGE_LOOP ( 'NONE', ( #12931, #13996, #3781, #10676 ) ) ;
#4331 = LINE ( 'NONE', #2031, #15067 ) ;
#4332 = PLANE ( 'NONE',  #1645 ) ;
#4333 = EDGE_CURVE ( 'NONE', #11968, #625, #11380, .T. ) ;
#4334 = VECTOR ( 'NONE', #11031, 1000.000000000000000 ) ;
#4335 = ADVANCED_FACE ( 'NONE', ( #836 ), #3308, .T. ) ;
#4336 = VECTOR ( 'NONE', #9451, 1000.000000000000000 ) ;
#4337 = CARTESIAN_POINT ( 'NONE',  ( 9.664560468771329127, -61.13673569060787827, -2.043233430234987935 ) ) ;
#4338 = CARTESIAN_POINT ( 'NONE',  ( 88.00000000000000000, 23.25070940071369208, 33.00000000000012790 ) ) ;
#4339 = CARTESIAN_POINT ( 'NONE',  ( 43.00000000000000711, 15.25070940071368497, -33.00000000000012790 ) ) ;
#4340 = CIRCLE ( 'NONE', #8301, 4.000000000000003553 ) ;
#4341 = DIRECTION ( 'NONE',  ( -0.000000000000000000, 0.000000000000000000, 1.000000000000000000 ) ) ;
#4342 = AXIS2_PLACEMENT_3D ( 'NONE', #3555, #9572, #12952 ) ;
#4343 = SPHERICAL_SURFACE ( 'NONE', #9694, 1.000000000000000000 ) ;
#4344 = CIRCLE ( 'NONE', #421, 0.7892041907098322762 ) ;
#4345 = LINE ( 'NONE', #12593, #5853 ) ;
#4346 = VERTEX_POINT ( 'NONE', #8002 ) ;
#4347 = CIRCLE ( 'NONE', #12975, 1.000000000000001998 ) ;
#4348 = CARTESIAN_POINT ( 'NONE',  ( 17.36157654472071599, -73.69234276600508338, -6.062089035220971311 ) ) ;
#4349 = ORIENTED_EDGE ( 'NONE', *, *, #1349, .F. ) ;
#4350 = CARTESIAN_POINT ( 'NONE',  ( -3.190546569013415379, 0.8906624217387615339, 57.50000000000012079 ) ) ;
#4351 = ORIENTED_EDGE ( 'NONE', *, *, #14436, .T. ) ;
#4352 = CARTESIAN_POINT ( 'NONE',  ( 12.91422301979531717, -63.78832907041026345, -4.037694147267451683 ) ) ;
#4353 = FACE_OUTER_BOUND ( 'NONE', #9221, .T. ) ;
#4354 = ORIENTED_EDGE ( 'NONE', *, *, #8670, .F. ) ;
#4355 = AXIS2_PLACEMENT_3D ( 'NONE', #12361, #649, #7590 ) ;
#4356 = MANIFOLD_SOLID_BREP ( 'Cut-Extrude1', #200 ) ;
#4357 = LINE ( 'NONE', #11275, #11956 ) ;
#4358 = LINE ( 'NONE', #12523, #8690 ) ;
#4359 = AXIS2_PLACEMENT_3D ( 'NONE', #11974, #2744, #366 ) ;
#4360 = VECTOR ( 'NONE', #1954, 1000.000000000000000 ) ;
#4361 = CARTESIAN_POINT ( 'NONE',  ( -3.190546569013415379, 0.8906624217387615339, -48.50000000000012079 ) ) ;
#4362 = AXIS2_PLACEMENT_3D ( 'NONE', #1695, #5021, #9725 ) ;
#4363 = ORIENTED_EDGE ( 'NONE', *, *, #12415, .F. ) ;
#4364 = EDGE_CURVE ( 'NONE', #11220, #14748, #9887, .T. ) ;
#4365 = CARTESIAN_POINT ( 'NONE',  ( 65.19224416878900286, -11.90459412701856756, 75.49439164730566176 ) ) ;
#4366 = CARTESIAN_POINT ( 'NONE',  ( 8.129701836179927810, -57.17378631614188578, -2.501045389182539935 ) ) ;
#4367 = CARTESIAN_POINT ( 'NONE',  ( -65.00000000000001421, -85.24929059928631148, 17.47499999999999787 ) ) ;
#4368 = DIRECTION ( 'NONE',  ( 0.000000000000000000, 1.000000000000000000, 0.000000000000000000 ) ) ;
#4369 = ORIENTED_EDGE ( 'NONE', *, *, #3054, .F. ) ;
#4370 = CIRCLE ( 'NONE', #12994, 0.7892041907098262810 ) ;
#4371 = VERTEX_POINT ( 'NONE', #4297 ) ;
#4372 = DIRECTION ( 'NONE',  ( -0.000000000000000000, -0.000000000000000000, 1.000000000000000000 ) ) ;
#4373 = ORIENTED_EDGE ( 'NONE', *, *, #9488, .F. ) ;
#4374 = CARTESIAN_POINT ( 'NONE',  ( 52.72873328492558187, -0.5014548242779810483, 48.51982618741349285 ) ) ;
#4375 = PRODUCT_DEFINITION_SHAPE ( 'NONE', 'NONE',  #9858 ) ;
#4376 = AXIS2_PLACEMENT_3D ( 'NONE', #10736, #8283, #3510 ) ;
#4377 = ORIENTED_EDGE ( 'NONE', *, *, #3105, .F. ) ;
#4378 = VERTEX_POINT ( 'NONE', #11617 ) ;
#4379 = CARTESIAN_POINT ( 'NONE',  ( 80.00000000000001421, -74.24929059928631148, -32.99999999999999289 ) ) ;
#4380 = CARTESIAN_POINT ( 'NONE',  ( -80.00000000000001421, -85.24929059928629727, 32.00000000000000000 ) ) ;
#4381 = ORIENTED_EDGE ( 'NONE', *, *, #7447, .F. ) ;
#4382 = EDGE_CURVE ( 'NONE', #13229, #7274, #2515, .T. ) ;
#4383 = DIRECTION ( 'NONE',  ( -0.4848096202550659650, -0.8746197071345572782, 0.000000000000000000 ) ) ;
#4384 = DIRECTION ( 'NONE',  ( 1.000000000000000000, 0.000000000000000000, 0.000000000000000000 ) ) ;
#4385 = EDGE_CURVE ( 'NONE', #2563, #6792, #3229, .T. ) ;
#4386 = ORIENTED_EDGE ( 'NONE', *, *, #14867, .F. ) ;
#4387 = CARTESIAN_POINT ( 'NONE',  ( 8.821484763567294607, -57.33450387999030795, 2.749014434309869248 ) ) ;
#4388 = CARTESIAN_POINT ( 'NONE',  ( 58.44010239582257071, -7.290881550929530164, 60.61639468829817190 ) ) ;
#4389 = DIRECTION ( 'NONE',  ( 1.000000000000000000, 0.000000000000000000, 0.000000000000000000 ) ) ;
#4390 = CARTESIAN_POINT ( 'NONE',  ( 23.47858629692699139, -53.24929059928630437, 6.492462156583989952 ) ) ;
#4391 = CARTESIAN_POINT ( 'NONE',  ( 32.59721271199144610, -59.08477032946249352, 2.725562014970989377 ) ) ;
#4392 = VERTEX_POINT ( 'NONE', #7933 ) ;
#4393 = CARTESIAN_POINT ( 'NONE',  ( 33.52366768382368889, -57.47994873761393819, 2.501453769636589275 ) ) ;
#4394 = CARTESIAN_POINT ( 'NONE',  ( 80.00000000000001421, -74.24929059928631148, 32.00000000000000000 ) ) ;
#4395 = ORIENTED_EDGE ( 'NONE', *, *, #882, .T. ) ;
#4396 = VERTEX_POINT ( 'NONE', #2149 ) ;
#4397 = CARTESIAN_POINT ( 'NONE',  ( -2.016677571526633510E-15, 23.25070940071368497, -33.00000000000012790 ) ) ;
#4398 = FACE_OUTER_BOUND ( 'NONE', #11661, .T. ) ;
#4399 = ORIENTED_EDGE ( 'NONE', *, *, #7253, .T. ) ;
#4400 = DIRECTION ( 'NONE',  ( 1.000000000000000000, 0.000000000000000000, 0.000000000000000000 ) ) ;
#4401 = CARTESIAN_POINT ( 'NONE',  ( 54.03086304124234829, 0.8903401505190762233, 62.84860122826521689 ) ) ;
#4402 = CARTESIAN_POINT ( 'NONE',  ( 80.00000000000001421, -72.24929059928631148, 34.99999999999999289 ) ) ;
#4403 = DIRECTION ( 'NONE',  ( 0.000000000000000000, -1.000000000000000000, 0.000000000000000000 ) ) ;
#4404 = VECTOR ( 'NONE', #5477, 1000.000000000000000 ) ;
#4405 = COLOUR_RGB ( '',0.7921568627450980005, 0.8196078431372548767, 0.9333333333333333481 ) ;
#4406 = CARTESIAN_POINT ( 'NONE',  ( -16.99999999999998579, -2.249290599286303927, 58.00000000000012079 ) ) ;
#4407 = ORIENTED_EDGE ( 'NONE', *, *, #14824, .F. ) ;
#4408 = CARTESIAN_POINT ( 'NONE',  ( 33.12582565096496268, -59.20619211347771937, 2.502190571104481176 ) ) ;
#4409 = VERTEX_POINT ( 'NONE', #7856 ) ;
#4410 = DIRECTION ( 'NONE',  ( 0.000000000000000000, 0.000000000000000000, 1.000000000000000000 ) ) ;
#4411 = LINE ( 'NONE', #9035, #13563 ) ;
#4412 = ORIENTED_EDGE ( 'NONE', *, *, #13506, .T. ) ;
#4413 = DIRECTION ( 'NONE',  ( 0.000000000000000000, 0.000000000000000000, 1.000000000000000000 ) ) ;
#4414 = CARTESIAN_POINT ( 'NONE',  ( 48.00000000000000711, 10.25070940071368497, 139.1143251403882459 ) ) ;
#4415 = EDGE_CURVE ( 'NONE', #7393, #4644, #6925, .T. ) ;
#4416 = CIRCLE ( 'NONE', #2953, 4.999999999999997335 ) ;
#4417 = CARTESIAN_POINT ( 'NONE',  ( 8.994667514334258485, -60.25563941105167487, -1.887923216546042449 ) ) ;
#4418 = DIRECTION ( 'NONE',  ( -0.000000000000000000, 1.000000000000000000, -0.000000000000000000 ) ) ;
#4419 = CARTESIAN_POINT ( 'NONE',  ( -16.99999999999998579, -2.249290599286303927, -38.50000000000012790 ) ) ;
#4420 = DIRECTION ( 'NONE',  ( -0.000000000000000000, 0.000000000000000000, 1.000000000000000000 ) ) ;
#4421 = CARTESIAN_POINT ( 'NONE',  ( -16.99999999999998579, -2.249290599286303927, 36.00000000000012079 ) ) ;
#4422 = DIRECTION ( 'NONE',  ( 1.000000000000000000, 0.000000000000000000, 0.000000000000000000 ) ) ;
#4423 = EDGE_CURVE ( 'NONE', #7757, #14061, #2074, .T. ) ;
#4424 = COLOUR_RGB ( '',0.7921568627450980005, 0.8196078431372548767, 0.9333333333333333481 ) ;
#4425 = ORIENTED_EDGE ( 'NONE', *, *, #1180, .F. ) ;
#4426 = ADVANCED_FACE ( 'NONE', ( #11529 ), #986, .F. ) ;
#4427 = DIRECTION ( 'NONE',  ( 0.000000000000000000, -1.000000000000000000, 0.000000000000000000 ) ) ;
#4428 = ORIENTED_EDGE ( 'NONE', *, *, #13345, .F. ) ;
#4429 = LINE ( 'NONE', #14821, #13782 ) ;
#4430 = ORIENTED_EDGE ( 'NONE', *, *, #691, .T. ) ;
#4431 = DIRECTION ( 'NONE',  ( 0.000000000000000000, 0.000000000000000000, 1.000000000000000000 ) ) ;
#4432 = DIRECTION ( 'NONE',  ( 0.000000000000000000, 0.000000000000000000, -1.000000000000000000 ) ) ;
#4433 = CIRCLE ( 'NONE', #12304, 4.505436745857433145 ) ;
#4434 = CARTESIAN_POINT ( 'NONE',  ( 69.28051765693513175, -4.295678830383773850, 77.19766410831374515 ) ) ;
#4435 = DIRECTION ( 'NONE',  ( -0.000000000000000000, -0.000000000000000000, -1.000000000000000000 ) ) ;
#4436 = CARTESIAN_POINT ( 'NONE',  ( 27.33509234239454244, -69.49659648540917090, -4.497058153269716918 ) ) ;
#4437 = ORIENTED_EDGE ( 'NONE', *, *, #9364, .T. ) ;
#4438 = CARTESIAN_POINT ( 'NONE',  ( 82.49066175147797253, 23.25070940071369208, 33.00000000000014211 ) ) ;
#4439 = CARTESIAN_POINT ( 'NONE',  ( 10.55748904889333772, -52.62785358159961646, -3.652922677138590757 ) ) ;
#4440 = DIRECTION ( 'NONE',  ( 0.000000000000000000, 0.000000000000000000, 1.000000000000000000 ) ) ;
#4441 = VECTOR ( 'NONE', #6738, 1000.000000000000000 ) ;
#4442 = DIRECTION ( 'NONE',  ( 0.000000000000000000, 0.000000000000000000, 1.000000000000000000 ) ) ;
#4443 = VERTEX_POINT ( 'NONE', #10395 ) ;
#4444 = AXIS2_PLACEMENT_3D ( 'NONE', #8867, #10964, #2806 ) ;
#4445 = FACE_OUTER_BOUND ( 'NONE', #6405, .T. ) ;
#4446 = ORIENTED_EDGE ( 'NONE', *, *, #11196, .F. ) ;
#4447 = CARTESIAN_POINT ( 'NONE',  ( -9.875903985900574611, 2.387222743937553293, 58.00000000000012079 ) ) ;
#4448 = ORIENTED_EDGE ( 'NONE', *, *, #11023, .F. ) ;
#4449 = EDGE_CURVE ( 'NONE', #13684, #9198, #8083, .T. ) ;
#4450 = VECTOR ( 'NONE', #2731, 1000.000000000000000 ) ;
#4451 = CARTESIAN_POINT ( 'NONE',  ( 9.539473796687049756, -61.03341231845509895, -2.731818205567035474 ) ) ;
#4452 = DIRECTION ( 'NONE',  ( 1.000000000000000000, -0.000000000000000000, 0.000000000000000000 ) ) ;
#4453 = ORIENTED_EDGE ( 'NONE', *, *, #3399, .F. ) ;
#4454 = AXIS2_PLACEMENT_3D ( 'NONE', #9061, #5373, #11209 ) ;
#4455 = VECTOR ( 'NONE', #11492, 1000.000000000000000 ) ;
#4456 = DIRECTION ( 'NONE',  ( 0.000000000000000000, 1.000000000000000000, 0.000000000000000000 ) ) ;
#4457 = DIRECTION ( 'NONE',  ( -1.000000000000000000, 0.000000000000000000, 0.000000000000000000 ) ) ;
#4458 = VERTEX_POINT ( 'NONE', #4018 ) ;
#4459 = DIRECTION ( 'NONE',  ( 0.000000000000000000, 0.000000000000000000, 1.000000000000000000 ) ) ;
#4460 = DIRECTION ( 'NONE',  ( 0.000000000000000000, 1.000000000000000000, -0.000000000000000000 ) ) ;
#4461 = FACE_OUTER_BOUND ( 'NONE', #653, .T. ) ;
#4462 = LINE ( 'NONE', #2236, #11283 ) ;
#4463 = VERTEX_POINT ( 'NONE', #1714 ) ;
#4464 = COLOUR_RGB ( '',0.7921568627450980005, 0.8196078431372548767, 0.9333333333333333481 ) ;
#4465 = CARTESIAN_POINT ( 'NONE',  ( 1.004339113574583608, 0.8906624217387615339, 57.50000000000012079 ) ) ;
#4466 = AXIS2_PLACEMENT_3D ( 'NONE', #7434, #12127, #572 ) ;
#4467 = VECTOR ( 'NONE', #10235, 1000.000000000000000 ) ;
#4468 = CARTESIAN_POINT ( 'NONE',  ( -9.035163663297472780, 1.943345362497546747, 48.01692658285808335 ) ) ;
#4469 = EDGE_CURVE ( 'NONE', #2463, #3805, #13807, .T. ) ;
#4470 = ORIENTED_EDGE ( 'NONE', *, *, #2256, .F. ) ;
#4471 = EDGE_CURVE ( 'NONE', #8897, #777, #10699, .T. ) ;
#4472 = FACE_OUTER_BOUND ( 'NONE', #9426, .T. ) ;
#4473 = DIRECTION ( 'NONE',  ( 0.000000000000000000, 0.000000000000000000, 1.000000000000000000 ) ) ;
#4474 = ORIENTED_EDGE ( 'NONE', *, *, #12230, .F. ) ;
#4475 = DIRECTION ( 'NONE',  ( 0.4848096202550659650, 0.8746197071345572782, 0.000000000000000000 ) ) ;
#4476 = CARTESIAN_POINT ( 'NONE',  ( 112.9262740340969060, 21.75070940071369918, -33.00000000000012790 ) ) ;
#4477 = EDGE_LOOP ( 'NONE', ( #1338, #9932, #8605, #3652, #689 ) ) ;
#4478 = DIRECTION ( 'NONE',  ( 0.8586863916854811096, -0.5125013958363124900, 0.000000000000000000 ) ) ;
#4479 = AXIS2_PLACEMENT_3D ( 'NONE', #10431, #10347, #4413 ) ;
#4480 = CARTESIAN_POINT ( 'NONE',  ( 32.52281604437752804, -59.06479067038041109, -2.757123406423310552 ) ) ;
#4481 = VECTOR ( 'NONE', #2514, 1000.000000000000000 ) ;
#4482 = AXIS2_PLACEMENT_3D ( 'NONE', #14023, #8414, #14183 ) ;
#4483 = DIRECTION ( 'NONE',  ( 0.000000000000000000, 0.000000000000000000, 1.000000000000000000 ) ) ;
#4484 = CARTESIAN_POINT ( 'NONE',  ( 30.63989068920077230, -53.42334933900650640, 3.800563870772192043 ) ) ;
#4485 = VECTOR ( 'NONE', #1141, 1000.000000000000000 ) ;
#4486 = DIRECTION ( 'NONE',  ( -0.5394184268574404584, 0.8420378618367728718, 0.000000000000000000 ) ) ;
#4487 = DIRECTION ( 'NONE',  ( -0.000000000000000000, 1.000000000000000000, 1.445602896647339163E-16 ) ) ;
#4488 = ORIENTED_EDGE ( 'NONE', *, *, #9810, .F. ) ;
#4489 = ADVANCED_FACE ( 'NONE', ( #88 ), #3767, .T. ) ;
#4490 = CARTESIAN_POINT ( 'NONE',  ( 32.36444917618072736, -60.82759157437160979, 1.965556376685483331 ) ) ;
#4491 = VECTOR ( 'NONE', #11885, 1000.000000000000000 ) ;
#4492 = EDGE_LOOP ( 'NONE', ( #14314, #14476, #3985, #51 ) ) ;
#4493 = CARTESIAN_POINT ( 'NONE',  ( 40.00000000000002132, -72.24929059928631148, 33.00000000000000000 ) ) ;
#4494 = DIRECTION ( 'NONE',  ( -0.2245798247307385087, 0.9744556954135528137, 0.000000000000000000 ) ) ;
#4495 = CIRCLE ( 'NONE', #3760, 10.46463184759104692 ) ;
#4496 = EDGE_LOOP ( 'NONE', ( #8466, #11675, #11635, #10550 ) ) ;
#4497 = CARTESIAN_POINT ( 'NONE',  ( 54.17164678268019173, 2.103670757168142114, 48.51982618741349285 ) ) ;
#4498 = FACE_OUTER_BOUND ( 'NONE', #3894, .T. ) ;
#4499 = VECTOR ( 'NONE', #473, 1000.000000000000000 ) ;
#4500 = CARTESIAN_POINT ( 'NONE',  ( 100.0000000000000284, 11.25070940071369563, 33.00000000000012790 ) ) ;
#4501 = DIRECTION ( 'NONE',  ( 0.8656763553493062036, 0.5006040828730242698, 0.000000000000000000 ) ) ;
#4502 = CARTESIAN_POINT ( 'NONE',  ( -65.00000000000001421, -87.24929059928631148, 22.49999999999999289 ) ) ;
#4503 = DIRECTION ( 'NONE',  ( -0.5394184268574404584, 0.8420378618367728718, 0.000000000000000000 ) ) ;
#4504 = CIRCLE ( 'NONE', #13120, 0.9999999999999991118 ) ;
#4505 = DIRECTION ( 'NONE',  ( 0.000000000000000000, 0.000000000000000000, 1.000000000000000000 ) ) ;
#4506 = DIRECTION ( 'NONE',  ( 0.000000000000000000, 1.000000000000000000, 0.000000000000000000 ) ) ;
#4507 = CIRCLE ( 'NONE', #13124, 2.524999999999999467 ) ;
#4508 = EDGE_LOOP ( 'NONE', ( #7540, #6040, #6962, #8539 ) ) ;
#4509 = CARTESIAN_POINT ( 'NONE',  ( 13.69731538040242746, -65.45139068073372357, -4.123085412756658741 ) ) ;
#4510 = ORIENTED_EDGE ( 'NONE', *, *, #12868, .F. ) ;
#4511 = CARTESIAN_POINT ( 'NONE',  ( 42.07846078193830408, 21.75070940071319114, -33.00000000000012790 ) ) ;
#4512 = VERTEX_POINT ( 'NONE', #14010 ) ;
#4513 = CARTESIAN_POINT ( 'NONE',  ( 11.45350991191545553, -61.78874994510978524, -3.497001979624778212 ) ) ;
#4514 = B_SPLINE_CURVE_WITH_KNOTS ( 'NONE', 3,
 ( #7355, #12044, #10904, #7433 ),
 .UNSPECIFIED., .F., .F.,
 ( 4, 4 ),
 ( 0.0005996816226312184136, 0.004245596575621797542 ),
 .UNSPECIFIED. ) ;
#4515 = EDGE_CURVE ( 'NONE', #8533, #9158, #2386, .T. ) ;
#4516 = CYLINDRICAL_SURFACE ( 'NONE', #8527, 2.000000000000000000 ) ;
#4517 = CARTESIAN_POINT ( 'NONE',  ( 0.000000000000000000, 2.750709400713692965, -33.00000000000012790 ) ) ;
#4518 = CARTESIAN_POINT ( 'NONE',  ( -8.787473001628837821, 2.499856724289235554, 58.00000000000012079 ) ) ;
#4519 = EDGE_CURVE ( 'NONE', #6001, #619, #3465, .T. ) ;
#4520 = ADVANCED_FACE ( 'NONE', ( #8326 ), #11847, .F. ) ;
#4521 = EDGE_CURVE ( 'NONE', #8826, #8112, #155, .T. ) ;
#4522 = ORIENTED_EDGE ( 'NONE', *, *, #1661, .F. ) ;
#4523 = CARTESIAN_POINT ( 'NONE',  ( 65.22735067928664421, -11.89594224596851468, 75.56344788988698724 ) ) ;
#4524 = CARTESIAN_POINT ( 'NONE',  ( 9.275519748983422019, -53.56780286158462445, -2.317958153236276964 ) ) ;
#4525 = DIRECTION ( 'NONE',  ( -0.000000000000000000, -0.000000000000000000, -1.000000000000000000 ) ) ;
#4526 = CARTESIAN_POINT ( 'NONE',  ( 35.49198652140812982, 21.75070940071315562, 33.00000000000012790 ) ) ;
#4527 = EDGE_CURVE ( 'NONE', #2895, #5118, #13468, .T. ) ;
#4528 = EDGE_LOOP ( 'NONE', ( #11682, #1049, #9936, #1912 ) ) ;
#4529 = ORIENTED_EDGE ( 'NONE', *, *, #6621, .T. ) ;
#4530 = DIRECTION ( 'NONE',  ( 1.000000000000000000, 0.000000000000000000, 0.000000000000000000 ) ) ;
#4531 = ORIENTED_EDGE ( 'NONE', *, *, #8059, .T. ) ;
#4532 = DIRECTION ( 'NONE',  ( -0.8208219420614848438, 0.4549890321264155046, 0.3453061251629924167 ) ) ;
#4533 = ORIENTED_EDGE ( 'NONE', *, *, #2745, .T. ) ;
#4534 = ORIENTED_EDGE ( 'NONE', *, *, #9772, .F. ) ;
#4535 = DIRECTION ( 'NONE',  ( -0.4848096202550659650, -0.8746197071345572782, -0.000000000000000000 ) ) ;
#4536 = DIRECTION ( 'NONE',  ( 1.000000000000000000, 0.000000000000000000, 0.000000000000000000 ) ) ;
#4537 = EDGE_CURVE ( 'NONE', #3899, #14177, #13016, .T. ) ;
#4538 = LINE ( 'NONE', #2229, #532 ) ;
#4539 = FILL_AREA_STYLE ('',( #12698 ) ) ;
#4540 = EDGE_LOOP ( 'NONE', ( #3612, #11674, #5172, #4213 ) ) ;
#4541 = DIRECTION ( 'NONE',  ( 0.000000000000000000, 0.000000000000000000, 1.000000000000000000 ) ) ;
#4542 = CARTESIAN_POINT ( 'NONE',  ( 114.6731053250840233, 21.75070940071369918, -33.00000000000012790 ) ) ;
#4543 = CARTESIAN_POINT ( 'NONE',  ( 33.58940973320519419, -55.84353942689658368, -1.893207994803262739 ) ) ;
#4544 = ADVANCED_FACE ( 'NONE', ( #8245 ), #297, .T. ) ;
#4545 = DIRECTION ( 'NONE',  ( 1.000000000000000000, 0.000000000000000000, 0.000000000000000000 ) ) ;
#4546 = CARTESIAN_POINT ( 'NONE',  ( 28.15716758062500702, -63.36896821088274123, 4.156457392287215669 ) ) ;
#4547 = EDGE_LOOP ( 'NONE', ( #14272, #13147, #6987, #3284 ) ) ;
#4548 = CARTESIAN_POINT ( 'NONE',  ( 69.40224406818397540, -3.449487665728846242, 71.39171174146984811 ) ) ;
#4549 = CARTESIAN_POINT ( 'NONE',  ( 55.36337191871069763, -7.136966431295542534, 60.61639468829817190 ) ) ;
#4550 = ORIENTED_EDGE ( 'NONE', *, *, #8059, .F. ) ;
#4551 = DIRECTION ( 'NONE',  ( -0.000000000000000000, 0.000000000000000000, -1.000000000000000000 ) ) ;
#4552 = CARTESIAN_POINT ( 'NONE',  ( 0.000000000000000000, 0.000000000000000000, 0.000000000000000000 ) ) ;
#4553 = LINE ( 'NONE', #4397, #7080 ) ;
#4554 = DIRECTION ( 'NONE',  ( 1.000000000000000000, 0.000000000000000000, 0.000000000000000000 ) ) ;
#4555 = EDGE_LOOP ( 'NONE', ( #12414, #6348, #1816 ) ) ;
#4556 = EDGE_CURVE ( 'NONE', #7720, #14080, #7232, .T. ) ;
#4557 = DIRECTION ( 'NONE',  ( 1.000000000000000000, 8.673617379884035472E-17, 0.000000000000000000 ) ) ;
#4558 = CARTESIAN_POINT ( 'NONE',  ( 82.49066175147797253, 23.25070940071369208, -33.00000000000012790 ) ) ;
#4559 = EDGE_CURVE ( 'NONE', #9532, #11054, #11437, .T. ) ;
#4560 = FACE_OUTER_BOUND ( 'NONE', #9113, .T. ) ;
#4561 = CARTESIAN_POINT ( 'NONE',  ( 32.37590170700519110, -54.69585338401581964, 3.125080077088496555 ) ) ;
#4562 = EDGE_CURVE ( 'NONE', #14878, #6522, #11336, .T. ) ;
#4563 = CARTESIAN_POINT ( 'NONE',  ( -16.99999999999998579, -12.24929059928630437, 38.00000000000012079 ) ) ;
#4564 = CARTESIAN_POINT ( 'NONE',  ( 59.00001739350650354, 10.75070940071368852, 84.20452624982236500 ) ) ;
#4565 = CLOSED_SHELL ( 'NONE', ( #14401, #2983, #11773, #12992, #2175, #8693, #5751, #7583, #8199, #8258, #7530, #14137, #10883, #11752, #3982, #9541, #1097, #6779, #3955, #6097, #10036, #12337, #8648, #1643, #9208, #1868, #13139, #8984, #12408, #15005, #2125, #1662, #6516, #7354, #6133, #8438, #15049, #10067, #2833, #6549, #8456, #851, #5358, #5372, #2592, #7165, #8476, #8835, #8548, #2721, #1797, #10299, #2795, #10668, #2707, #6497, #10626, #13589, #10510, #14716, #6637, #12508, #3430, #12820, #13223, #3743, #14418, #8287, #202, #4809, #12520, #4426, #3649, #12462, #5082, #13809, #3790, #9474, #11976, #3862, #10790, #12253, #4307, #10167, #6316, #10370, #15201, #13369, #1621, #11925, #13628, #8590, #2559, #9235, #12482, #3651, #8660, #13463, #13461, #1952 ) ) ;
#4566 = ORIENTED_EDGE ( 'NONE', *, *, #1579, .F. ) ;
#4567 = VECTOR ( 'NONE', #10183, 1000.000000000000000 ) ;
#4568 = CARTESIAN_POINT ( 'NONE',  ( 32.10922531551839398, -61.48375833294921478, -2.718831331512520322 ) ) ;
#4569 = EDGE_LOOP ( 'NONE', ( #8733, #7130, #2531, #9448 ) ) ;
#4570 = CARTESIAN_POINT ( 'NONE',  ( 104.9938193859979236, 0.000000000000000000, 139.1143251403882459 ) ) ;
#4571 = DIRECTION ( 'NONE',  ( 0.000000000000000000, 0.000000000000000000, -1.000000000000000000 ) ) ;
#4572 = ORIENTED_EDGE ( 'NONE', *, *, #9117, .T. ) ;
#4573 = DIRECTION ( 'NONE',  ( -1.000000000000000000, 0.000000000000000000, 0.000000000000000000 ) ) ;
#4574 = FACE_OUTER_BOUND ( 'NONE', #11764, .T. ) ;
#4575 = CARTESIAN_POINT ( 'NONE',  ( 13.77965687262195260, -67.87804980504323282, 4.252496648654521039 ) ) ;
#4576 = EDGE_CURVE ( 'NONE', #12374, #13613, #10776, .T. ) ;
#4577 = EDGE_CURVE ( 'NONE', #341, #2589, #10468, .T. ) ;
#4578 = LINE ( 'NONE', #13893, #13953 ) ;
#4579 = FACE_OUTER_BOUND ( 'NONE', #1220, .T. ) ;
#4580 = DIRECTION ( 'NONE',  ( -0.4848096202550660205, -0.8746197071345573892, 0.000000000000000000 ) ) ;
#4581 = LINE ( 'NONE', #9281, #3773 ) ;
#4582 = CARTESIAN_POINT ( 'NONE',  ( 13.86173033120691223, -69.39711819508849544, 2.500000000000000000 ) ) ;
#4583 = EDGE_LOOP ( 'NONE', ( #4116, #1006, #13937, #13292 ) ) ;
#4584 = CARTESIAN_POINT ( 'NONE',  ( 6.988058422621596932, -48.72530132304424910, -2.733088102048180978 ) ) ;
#4585 = ORIENTED_EDGE ( 'NONE', *, *, #8487, .T. ) ;
#4586 = CARTESIAN_POINT ( 'NONE',  ( 61.57781019154727176, -5.828480965243416634, 48.51982618741349285 ) ) ;
#4587 = CIRCLE ( 'NONE', #6305, 4.194885682588113340 ) ;
#4588 = ORIENTED_EDGE ( 'NONE', *, *, #14888, .F. ) ;
#4589 = CARTESIAN_POINT ( 'NONE',  ( -3.190546569013415379, 0.8906624217387615339, 48.50000000000012079 ) ) ;
#4590 =( NAMED_UNIT ( * ) SI_UNIT ( $, .STERADIAN. ) SOLID_ANGLE_UNIT ( ) );
#4591 = CARTESIAN_POINT ( 'NONE',  ( 18.08359295236611786, -58.63441909321038281, -6.426091441073433330 ) ) ;
#4592 = CARTESIAN_POINT ( 'NONE',  ( 80.00000000000001421, -74.24929059928631148, 4.000000000000000000 ) ) ;
#4593 = VECTOR ( 'NONE', #8235, 1000.000000000000000 ) ;
#4594 =( GEOMETRIC_REPRESENTATION_CONTEXT ( 3 ) GLOBAL_UNCERTAINTY_ASSIGNED_CONTEXT ( ( #6893 ) ) GLOBAL_UNIT_ASSIGNED_CONTEXT ( ( #1493, #13402, #10888 ) ) REPRESENTATION_CONTEXT ( 'NONE', 'WORKASPACE' ) );
#4595 = VERTEX_POINT ( 'NONE', #9313 ) ;
#4596 = VECTOR ( 'NONE', #11001, 1000.000000000000000 ) ;
#4597 = AXIS2_PLACEMENT_3D ( 'NONE', #8206, #9668, #5897 ) ;
#4598 = DIRECTION ( 'NONE',  ( 0.000000000000000000, 0.000000000000000000, 1.000000000000000000 ) ) ;
#4599 = CARTESIAN_POINT ( 'NONE',  ( 8.097303543835579376, -56.24990207478561643, -2.565511669097837455 ) ) ;
#4600 = CARTESIAN_POINT ( 'NONE',  ( 58.00000000000000711, -2.249290599286309256, 82.40005259842790508 ) ) ;
#4601 = EDGE_CURVE ( 'NONE', #3165, #8619, #8423, .T. ) ;
#4602 = LINE ( 'NONE', #12533, #9696 ) ;
#4603 = VERTEX_POINT ( 'NONE', #5005 ) ;
#4604 = ORIENTED_EDGE ( 'NONE', *, *, #1813, .T. ) ;
#4605 = CARTESIAN_POINT ( 'NONE',  ( -6.999999999999987566, -2.249290599286443815, -32.99999999999987921 ) ) ;
#4606 = ORIENTED_EDGE ( 'NONE', *, *, #3292, .T. ) ;
#4607 = DIRECTION ( 'NONE',  ( -0.000000000000000000, -0.000000000000000000, -1.000000000000000000 ) ) ;
#4608 = CIRCLE ( 'NONE', #13217, 0.9999999999999996669 ) ;
#4609 = ORIENTED_EDGE ( 'NONE', *, *, #12041, .T. ) ;
#4610 = VECTOR ( 'NONE', #1150, 1000.000000000000000 ) ;
#4611 = VERTEX_POINT ( 'NONE', #6166 ) ;
#4612 = ADVANCED_FACE ( 'NONE', ( #10851 ), #5733, .F. ) ;
#4613 = CIRCLE ( 'NONE', #12475, 7.000000000000000000 ) ;
#4614 = DIRECTION ( 'NONE',  ( 1.000000000000000000, -0.000000000000000000, 0.000000000000000000 ) ) ;
#4615 = PLANE ( 'NONE',  #1288 ) ;
#4616 = EDGE_CURVE ( 'NONE', #10292, #9229, #5717, .T. ) ;
#4617 = EDGE_CURVE ( 'NONE', #6145, #612, #2767, .T. ) ;
#4618 = CARTESIAN_POINT ( 'NONE',  ( 80.00000000000001421, -74.24929059928631148, -32.00000000000000000 ) ) ;
#4619 = DIRECTION ( 'NONE',  ( -0.000000000000000000, 1.000000000000000000, -1.927470528863119788E-16 ) ) ;
#4620 = VERTEX_POINT ( 'NONE', #14863 ) ;
#4621 = VECTOR ( 'NONE', #461, 1000.000000000000000 ) ;
#4622 = CARTESIAN_POINT ( 'NONE',  ( 80.00000000000001421, -76.24929059928631148, -4.000000000000000000 ) ) ;
#4623 = FACE_OUTER_BOUND ( 'NONE', #1524, .T. ) ;
#4624 = CARTESIAN_POINT ( 'NONE',  ( 72.24825649497627467, -14.72064441357683684, 73.07464432123546771 ) ) ;
#4625 = CARTESIAN_POINT ( 'NONE',  ( 23.59140218558529867, -57.03285117761353717, 6.445925775545360281 ) ) ;
#4626 = AXIS2_PLACEMENT_3D ( 'NONE', #4401, #3643, #7104 ) ;
#4627 = VERTEX_POINT ( 'NONE', #9183 ) ;
#4628 = CARTESIAN_POINT ( 'NONE',  ( 12.36791015745245836, -52.24929059928631148, 3.199931146564429341 ) ) ;
#4629 = EDGE_CURVE ( 'NONE', #14228, #1441, #10415, .T. ) ;
#4630 = EDGE_CURVE ( 'NONE', #6102, #8969, #15105, .T. ) ;
#4631 = EDGE_LOOP ( 'NONE', ( #11438, #13264 ) ) ;
#4632 = FACE_OUTER_BOUND ( 'NONE', #8135, .T. ) ;
#4633 = SURFACE_STYLE_FILL_AREA ( #12881 ) ;
#4634 = CARTESIAN_POINT ( 'NONE',  ( 0.000000000000000000, 0.000000000000000000, 0.000000000000000000 ) ) ;
#4635 = CARTESIAN_POINT ( 'NONE',  ( 8.201103799357259305, -57.48563641131178770, 1.816685854991402893 ) ) ;
#4636 = LINE ( 'NONE', #5955, #15057 ) ;
#4637 = ORIENTED_EDGE ( 'NONE', *, *, #9454, .F. ) ;
#4638 = LINE ( 'NONE', #9019, #8728 ) ;
#4639 = CARTESIAN_POINT ( 'NONE',  ( 108.0866310645538562, 0.000000000000000000, 139.1143251403882459 ) ) ;
#4640 = CARTESIAN_POINT ( 'NONE',  ( 8.873138538923161178, -60.06401564186453612, 1.862089353234911204 ) ) ;
#4641 = DIRECTION ( 'NONE',  ( -0.000000000000000000, 1.000000000000000000, 0.000000000000000000 ) ) ;
#4642 = CARTESIAN_POINT ( 'NONE',  ( 12.36791015745245836, -52.24929059928631148, -3.199931146564426232 ) ) ;
#4643 = LINE ( 'NONE', #863, #6660 ) ;
#4644 = VERTEX_POINT ( 'NONE', #4476 ) ;
#4645 = DIRECTION ( 'NONE',  ( 0.8746197071345573892, -0.4848096202550657430, 0.000000000000000000 ) ) ;
#4646 = VERTEX_POINT ( 'NONE', #8021 ) ;
#4647 = CARTESIAN_POINT ( 'NONE',  ( 70.26445833701072274, -4.474174595298148205, 71.19766410831374515 ) ) ;
#4648 = DIRECTION ( 'NONE',  ( 0.000000000000000000, 0.000000000000000000, 1.000000000000000000 ) ) ;
#4649 = B_SPLINE_CURVE_WITH_KNOTS ( 'NONE', 3,
 ( #14770, #6326, #469, #5312, #396, #14618, #12098, #1625, #8847, #14551, #2708, #3010 ),
 .UNSPECIFIED., .F., .F.,
 ( 4, 2, 2, 2, 2, 4 ),
 ( 0.000000000000000000, 0.001071381053236907443, 0.002142762106473816621, 0.003214143159710726016, 0.003749833686329184183, 0.004285524212947642783 ),
 .UNSPECIFIED. ) ;
#4650 = ORIENTED_EDGE ( 'NONE', *, *, #11318, .F. ) ;
#4651 = DIRECTION ( 'NONE',  ( 1.000000000000000000, 0.000000000000000000, 0.000000000000000000 ) ) ;
#4652 = CYLINDRICAL_SURFACE ( 'NONE', #10749, 0.7892041907098262810 ) ;
#4653 = EDGE_CURVE ( 'NONE', #9290, #9928, #14788, .T. ) ;
#4654 = DIRECTION ( 'NONE',  ( 0.000000000000000000, 0.000000000000000000, 1.000000000000000000 ) ) ;
#4655 = EDGE_CURVE ( 'NONE', #8078, #7393, #5407, .T. ) ;
#4656 = VECTOR ( 'NONE', #2789, 1000.000000000000000 ) ;
#4657 = CIRCLE ( 'NONE', #10058, 0.5000000000000001110 ) ;
#4658 = LINE ( 'NONE', #1107, #10516 ) ;
#4659 = DIRECTION ( 'NONE',  ( 0.000000000000000000, -0.000000000000000000, -1.000000000000000000 ) ) ;
#4660 = CARTESIAN_POINT ( 'NONE',  ( 122.6668124272373745, -38.09469005714606737, 52.68020260152229639 ) ) ;
#4661 = CARTESIAN_POINT ( 'NONE',  ( 63.36453054171181520, -0.8129776999179910701, 48.51982618741349285 ) ) ;
#4662 = CARTESIAN_POINT ( 'NONE',  ( 32.39494368350905518, -53.50439862579374761, 3.186601206341092674 ) ) ;
#4663 = EDGE_LOOP ( 'NONE', ( #14324, #9179, #677 ) ) ;
#4664 = CARTESIAN_POINT ( 'NONE',  ( 13.56629308258002098, -63.36896821090397225, -4.156457390613502945 ) ) ;
#4665 = VERTEX_POINT ( 'NONE', #4313 ) ;
#4666 = AXIS2_PLACEMENT_3D ( 'NONE', #15168, #10475, #8009 ) ;
#4667 = CARTESIAN_POINT ( 'NONE',  ( 58.00000000000000711, -2.249290599286311032, -33.00000000000012790 ) ) ;
#4668 = AXIS2_PLACEMENT_3D ( 'NONE', #14874, #3263, #5740 ) ;
#4669 = ORIENTED_EDGE ( 'NONE', *, *, #580, .F. ) ;
#4670 = ORIENTED_EDGE ( 'NONE', *, *, #4562, .F. ) ;
#4671 = CARTESIAN_POINT ( 'NONE',  ( 64.62474033849325394, -11.62473885758638303, 75.37908211999966568 ) ) ;
#4672 = FACE_OUTER_BOUND ( 'NONE', #8334, .T. ) ;
#4673 = EDGE_CURVE ( 'NONE', #1961, #7398, #13817, .T. ) ;
#4674 = CARTESIAN_POINT ( 'NONE',  ( -16.99999999999998579, -2.249290599286303927, -58.00000000000012079 ) ) ;
#4675 = VERTEX_POINT ( 'NONE', #11547 ) ;
#4676 = VERTEX_POINT ( 'NONE', #13948 ) ;
#4677 = VECTOR ( 'NONE', #11390, 1000.000000000000000 ) ;
#4678 = CARTESIAN_POINT ( 'NONE',  ( 8.201103799357259305, -57.48563641131178770, -1.816685854991388682 ) ) ;
#4679 = LINE ( 'NONE', #9376, #3148 ) ;
#4680 = FACE_OUTER_BOUND ( 'NONE', #3515, .T. ) ;
#4681 = LINE ( 'NONE', #13682, #6092 ) ;
#4682 = ORIENTED_EDGE ( 'NONE', *, *, #10425, .F. ) ;
#4683 = ORIENTED_EDGE ( 'NONE', *, *, #12171, .F. ) ;
#4684 = DIRECTION ( 'NONE',  ( 0.8208219420614786266, -0.4549890321264268289, -0.3453061251629919726 ) ) ;
#4685 = EDGE_LOOP ( 'NONE', ( #8803, #6903, #3415, #10373 ) ) ;
#4686 = CARTESIAN_POINT ( 'NONE',  ( 62.50543674585744469, -2.249290599286311032, 36.00000000000012079 ) ) ;
#4687 = ORIENTED_EDGE ( 'NONE', *, *, #2672, .T. ) ;
#4688 = EDGE_CURVE ( 'NONE', #14170, #9032, #11314, .T. ) ;
#4689 = ORIENTED_EDGE ( 'NONE', *, *, #6317, .F. ) ;
#4690 = DIRECTION ( 'NONE',  ( 1.000000000000000000, 0.000000000000000000, 0.000000000000000000 ) ) ;
#4691 = CARTESIAN_POINT ( 'NONE',  ( 20.86173033120691045, -96.56299909827106376, 0.000000000000000000 ) ) ;
#4692 = FACE_OUTER_BOUND ( 'NONE', #5342, .T. ) ;
#4693 = PRODUCT_DEFINITION_SHAPE ( 'NONE', 'NONE',  #11824 ) ;
#4694 = DIRECTION ( 'NONE',  ( 0.8746197071345571672, -0.4848096202550662981, 0.000000000000000000 ) ) ;
#4695 = EDGE_LOOP ( 'NONE', ( #12254, #10078, #7711, #7351 ) ) ;
#4696 =( BOUNDED_SURFACE ( )  B_SPLINE_SURFACE ( 3, 2, ( 
 ( #4255, #3337, #13572 ),
 ( #5575, #13728, #3103 ),
 ( #1944, #12416, #10344 ),
 ( #3041, #12652, #12347 ) ),
 .UNSPECIFIED., .F., .F., .F. ) 
 B_SPLINE_SURFACE_WITH_KNOTS ( ( 4, 4 ),
 ( 3, 3 ),
 ( 3.469446951953614189E-18, 0.006683255761480919911 ),
 ( 0.000000000000000000, 1.000000000000000000 ),
 .UNSPECIFIED. ) 
 GEOMETRIC_REPRESENTATION_ITEM ( )  RATIONAL_B_SPLINE_SURFACE ( (
 ( 1.000000000000000000, 0.7071067811865500152, 1.000000000000000000),
 ( 1.000000000000000000, 0.7035788727800790232, 1.000000000000000000),
 ( 1.000000000000000000, 0.6996284196041374637, 1.000000000000000000),
 ( 1.000000000000000000, 0.6947298545087537969, 1.000000000000000000) ) ) 
 REPRESENTATION_ITEM ( '' )  SURFACE ( )  );
#4697 = CIRCLE ( 'NONE', #1501, 4.000000000000003553 ) ;
#4698 = DIRECTION ( 'NONE',  ( 0.000000000000000000, 0.000000000000000000, 1.000000000000000000 ) ) ;
#4699 = DIRECTION ( 'NONE',  ( 0.000000000000000000, 0.000000000000000000, 1.000000000000000000 ) ) ;
#4700 = ADVANCED_FACE ( 'NONE', ( #4398 ), #6706, .F. ) ;
#4701 = DIRECTION ( 'NONE',  ( -0.000000000000000000, 0.000000000000000000, 1.000000000000000000 ) ) ;
#4702 = CARTESIAN_POINT ( 'NONE',  ( -16.99999999999998579, -2.249290599286303927, -50.00000000000012079 ) ) ;
#4703 = ORIENTED_EDGE ( 'NONE', *, *, #1705, .T. ) ;
#4704 = DIRECTION ( 'NONE',  ( -0.000000000000000000, -0.000000000000000000, -1.000000000000000000 ) ) ;
#4705 = AXIS2_PLACEMENT_3D ( 'NONE', #14154, #11835, #6996 ) ;
#4706 = ORIENTED_EDGE ( 'NONE', *, *, #4933, .F. ) ;
#4707 = FACE_OUTER_BOUND ( 'NONE', #10747, .T. ) ;
#4708 = FACE_OUTER_BOUND ( 'NONE', #1940, .T. ) ;
#4709 = TOROIDAL_SURFACE ( 'NONE', #6911, 9.500000000000001776, 0.5000000000000000000 ) ;
#4710 = B_SPLINE_CURVE_WITH_KNOTS ( 'NONE', 3,
 ( #188, #1188, #11800, #1258, #3499, #8201 ),
 .UNSPECIFIED., .F., .F.,
 ( 4, 2, 4 ),
 ( 0.001000432843099107339, 0.009082381923694659437, 0.01716433100429023278 ),
 .UNSPECIFIED. ) ;
#4711 = CARTESIAN_POINT ( 'NONE',  ( -11.57001547143821085, -9.459140135624386048, -48.26605223432068925 ) ) ;
#4712 = CARTESIAN_POINT ( 'NONE',  ( 98.40734512546775647, 23.25070940071369208, 33.00000000000012790 ) ) ;
#4713 = ORIENTED_EDGE ( 'NONE', *, *, #10946, .T. ) ;
#4714 = LINE ( 'NONE', #9414, #13176 ) ;
#4715 = DIRECTION ( 'NONE',  ( 0.000000000000000000, 0.000000000000000000, -1.000000000000000000 ) ) ;
#4716 = EDGE_CURVE ( 'NONE', #11141, #8798, #6782, .T. ) ;
#4717 = EDGE_CURVE ( 'NONE', #170, #7490, #310, .T. ) ;
#4718 = EDGE_CURVE ( 'NONE', #14789, #60, #10881, .T. ) ;
#4719 = VECTOR ( 'NONE', #1723, 1000.000000000000000 ) ;
#4720 = DIRECTION ( 'NONE',  ( 0.8656763553492632379, 0.5006040828730989878, 1.736819309459606431E-15 ) ) ;
#4721 = VECTOR ( 'NONE', #8325, 1000.000000000000000 ) ;
#4722 = DIRECTION ( 'NONE',  ( -0.5394184268574385710, 0.8420378618367740930, 0.000000000000000000 ) ) ;
#4723 = DIRECTION ( 'NONE',  ( -0.8208219420614786266, 0.4549890321264268289, 0.3453061251629919726 ) ) ;
#4724 = AXIS2_PLACEMENT_3D ( 'NONE', #1380, #6086, #5936 ) ;
#4725 = ORIENTED_EDGE ( 'NONE', *, *, #15129, .T. ) ;
#4726 = ADVANCED_FACE ( 'NONE', ( #1008 ), #5491, .F. ) ;
#4727 = EDGE_LOOP ( 'NONE', ( #2420, #10789, #13026, #6753 ) ) ;
#4728 = CARTESIAN_POINT ( 'NONE',  ( -21.58505662828840244, 4.908031226326156293, 58.00000000000012079 ) ) ;
#4729 = VERTEX_POINT ( 'NONE', #6944 ) ;
#4730 = CARTESIAN_POINT ( 'NONE',  ( -22.16581936427349575, -2.249290599286304371, -58.00000000000012079 ) ) ;
#4731 = CYLINDRICAL_SURFACE ( 'NONE', #12336, 8.924024642120684803 ) ;
#4732 = VECTOR ( 'NONE', #8093, 1000.000000000000000 ) ;
#4733 = DIRECTION ( 'NONE',  ( -0.000000000000000000, 1.000000000000000000, 1.445602896647339163E-16 ) ) ;
#4734 = DIRECTION ( 'NONE',  ( 0.8746197071345569451, -0.4848096202550666312, 0.000000000000000000 ) ) ;
#4735 = VECTOR ( 'NONE', #1584, 1000.000000000000000 ) ;
#4736 = AXIS2_PLACEMENT_3D ( 'NONE', #930, #10331, #2327 ) ;
#4737 = CARTESIAN_POINT ( 'NONE',  ( 14.31939787082484727, -67.79239290436629517, 4.531617596076316090 ) ) ;
#4738 = AXIS2_PLACEMENT_3D ( 'NONE', #9923, #12294, #9707 ) ;
#4739 = FACE_BOUND ( 'NONE', #10322, .T. ) ;
#4740 = DIRECTION ( 'NONE',  ( -1.000000000000000000, -9.912705577010325549E-17, 0.000000000000000000 ) ) ;
#4741 = FACE_OUTER_BOUND ( 'NONE', #4477, .T. ) ;
#4742 = DIRECTION ( 'NONE',  ( 0.000000000000000000, -1.000000000000000000, 0.000000000000000000 ) ) ;
#4743 = VECTOR ( 'NONE', #14648, 1000.000000000000000 ) ;
#4744 = EDGE_CURVE ( 'NONE', #2756, #5424, #3747, .T. ) ;
#4745 = CARTESIAN_POINT ( 'NONE',  ( 30.62910135305399351, -53.42013688713479524, 3.804487959019970056 ) ) ;
#4746 = ORIENTED_EDGE ( 'NONE', *, *, #13449, .F. ) ;
#4747 = CARTESIAN_POINT ( 'NONE',  ( 13.86173033120691223, -69.39711819508849544, 2.500000000000000000 ) ) ;
#4748 = PRODUCT_DEFINITION_CONTEXT ( 'detailed design', #2001, 'design' ) ;
#4749 = VECTOR ( 'NONE', #7283, 1000.000000000000000 ) ;
#4750 = ORIENTED_EDGE ( 'NONE', *, *, #13281, .F. ) ;
#4751 = DIRECTION ( 'NONE',  ( 1.000000000000000000, 0.000000000000000000, 0.000000000000000000 ) ) ;
#4752 = ORIENTED_EDGE ( 'NONE', *, *, #5951, .T. ) ;
#4753 = VERTEX_POINT ( 'NONE', #12486 ) ;
#4754 = CARTESIAN_POINT ( 'NONE',  ( 64.97069784687126059, -11.35197416150241523, 76.94490957099723971 ) ) ;
#4755 = CARTESIAN_POINT ( 'NONE',  ( 58.00000000000000711, -2.249290599286309256, 81.40005259842790508 ) ) ;
#4756 = DIRECTION ( 'NONE',  ( 0.000000000000000000, -1.000000000000000000, 0.000000000000000000 ) ) ;
#4757 = AXIS2_PLACEMENT_3D ( 'NONE', #12137, #11048, #1592 ) ;
#4758 = ORIENTED_EDGE ( 'NONE', *, *, #667, .T. ) ;
#4759 = VECTOR ( 'NONE', #3989, 1000.000000000000000 ) ;
#4760 = CARTESIAN_POINT ( 'NONE',  ( 20.86173033120691045, -87.24929059928631148, 0.000000000000000000 ) ) ;
#4761 = DIRECTION ( 'NONE',  ( 0.000000000000000000, 0.000000000000000000, 1.000000000000000000 ) ) ;
#4762 = ADVANCED_FACE ( 'NONE', ( #4242 ), #1933, .T. ) ;
#4763 = EDGE_CURVE ( 'NONE', #3352, #11220, #14328, .T. ) ;
#4764 = CARTESIAN_POINT ( 'NONE',  ( 98.40734512546775647, 23.25070940071369208, 139.1143251403882459 ) ) ;
#4765 = VERTEX_POINT ( 'NONE', #3171 ) ;
#4766 = ORIENTED_EDGE ( 'NONE', *, *, #3813, .T. ) ;
#4767 = CARTESIAN_POINT ( 'NONE',  ( -0.9277479332649583021, -2.641590149077306826, -57.50000000000012079 ) ) ;
#4768 = ORIENTED_EDGE ( 'NONE', *, *, #7999, .F. ) ;
#4769 = CARTESIAN_POINT ( 'NONE',  ( 10.23047706855496308, -60.71197230342421136, -3.050751728647428607 ) ) ;
#4770 = ORIENTED_EDGE ( 'NONE', *, *, #5411, .F. ) ;
#4771 = ORIENTED_EDGE ( 'NONE', *, *, #7741, .F. ) ;
#4772 = AXIS2_PLACEMENT_3D ( 'NONE', #1967, #13522, #2989 ) ;
#4773 = DIRECTION ( 'NONE',  ( 0.000000000000000000, 0.000000000000000000, 1.000000000000000000 ) ) ;
#4774 = FACE_OUTER_BOUND ( 'NONE', #6720, .T. ) ;
#4775 = ORIENTED_EDGE ( 'NONE', *, *, #2324, .F. ) ;
#4776 = CARTESIAN_POINT ( 'NONE',  ( 25.17145219045130489, -52.24929059928630437, -4.731961142181946300 ) ) ;
#4777 = CARTESIAN_POINT ( 'NONE',  ( 25.81270058232203013, 0.000000000000000000, 139.1143251403882459 ) ) ;
#4778 = ORIENTED_EDGE ( 'NONE', *, *, #9015, .T. ) ;
#4779 = ADVANCED_FACE ( 'NONE', ( #2009 ), #12641, .F. ) ;
#4780 = CARTESIAN_POINT ( 'NONE',  ( -20.99999999999998579, -2.249290599286303483, -38.00000000000012079 ) ) ;
#4781 = CARTESIAN_POINT ( 'NONE',  ( -9.101643754575787781, 2.066879234150345024, -47.52815511422343775 ) ) ;
#4782 = EDGE_CURVE ( 'NONE', #12049, #12792, #7193, .T. ) ;
#4783 = DIRECTION ( 'NONE',  ( 1.000000000000000000, 0.000000000000000000, 0.000000000000000000 ) ) ;
#4784 = ORIENTED_EDGE ( 'NONE', *, *, #11562, .T. ) ;
#4785 = CARTESIAN_POINT ( 'NONE',  ( 69.32502553878046569, -4.050333426515871693, 71.19766411846617871 ) ) ;
#4786 = VERTEX_POINT ( 'NONE', #2629 ) ;
#4787 = CARTESIAN_POINT ( 'NONE',  ( 65.00000000000001421, -85.24929059928631148, 19.99999999999999645 ) ) ;
#4788 = ORIENTED_EDGE ( 'NONE', *, *, #14249, .F. ) ;
#4789 = SHAPE_REPRESENTATION_RELATIONSHIP ( 'NONE' , 'NONE' ,  #8914, #419 ) ;
#4790 = CARTESIAN_POINT ( 'NONE',  ( 8.597635011448856446, -59.20619211347771937, 2.502190571104474959 ) ) ;
#4791 = CARTESIAN_POINT ( 'NONE',  ( -3.285520523750506516, 5.681530634152946568, -48.00000000000012079 ) ) ;
#4792 = EDGE_LOOP ( 'NONE', ( #4935, #12146, #8015, #14909 ) ) ;
#4793 = CARTESIAN_POINT ( 'NONE',  ( -8.982583014919022446, 1.839844381040865562, -48.00000000000012079 ) ) ;
#4794 = EDGE_CURVE ( 'NONE', #12049, #11720, #4636, .T. ) ;
#4795 = DIRECTION ( 'NONE',  ( 1.000000000000000000, 0.000000000000000000, 0.000000000000000000 ) ) ;
#4796 = DIRECTION ( 'NONE',  ( 0.000000000000000000, 1.000000000000000000, -0.000000000000000000 ) ) ;
#4797 = CARTESIAN_POINT ( 'NONE',  ( 32.86846178545243902, -54.08202937160073986, 2.181355823101601477 ) ) ;
#4798 = CARTESIAN_POINT ( 'NONE',  ( 32.50723669307611630, -54.89772082965748012, -3.066133849897850983 ) ) ;
#4799 = EDGE_CURVE ( 'NONE', #8184, #11541, #105, .T. ) ;
#4800 = ORIENTED_EDGE ( 'NONE', *, *, #10449, .T. ) ;
#4801 = DIRECTION ( 'NONE',  ( -0.000000000000000000, 0.000000000000000000, 1.000000000000000000 ) ) ;
#4802 = ORIENTED_EDGE ( 'NONE', *, *, #12107, .T. ) ;
#4803 = DIRECTION ( 'NONE',  ( -0.000000000000000000, -0.000000000000000000, -1.000000000000000000 ) ) ;
#4804 = CARTESIAN_POINT ( 'NONE',  ( 58.00000000000000711, -2.249290599286309256, 82.40005259842790508 ) ) ;
#4805 = ORIENTED_EDGE ( 'NONE', *, *, #1604, .F. ) ;
#4806 = CARTESIAN_POINT ( 'NONE',  ( 62.88869237673507229, 0.3854521819929429549, 54.56811043785582882 ) ) ;
#4807 = DIRECTION ( 'NONE',  ( -0.000000000000000000, 0.000000000000000000, -1.000000000000000000 ) ) ;
#4808 = CARTESIAN_POINT ( 'NONE',  ( 70.17072936512437309, -3.859920535181831980, 76.07070489651268019 ) ) ;
#4809 = ADVANCED_FACE ( 'NONE', ( #9332 ), #7019, .F. ) ;
#4810 = LINE ( 'NONE', #7040, #4126 ) ;
#4811 = FACE_OUTER_BOUND ( 'NONE', #9991, .T. ) ;
#4812 = AXIS2_PLACEMENT_3D ( 'NONE', #8624, #1558, #12167 ) ;
#4813 = CARTESIAN_POINT ( 'NONE',  ( 62.32645299789339788, 5.555837219666858395, 48.51982618741349285 ) ) ;
#4814 = VECTOR ( 'NONE', #15183, 1000.000000000000000 ) ;
#4815 = CARTESIAN_POINT ( 'NONE',  ( 32.09796538084800943, -53.24070755262462740, 2.425727701578423989 ) ) ;
#4816 = VERTEX_POINT ( 'NONE', #4712 ) ;
#4817 = FACE_BOUND ( 'NONE', #12208, .T. ) ;
#4818 = ORIENTED_EDGE ( 'NONE', *, *, #14852, .F. ) ;
#4819 = ADVANCED_FACE ( 'NONE', ( #254 ), #14338, .T. ) ;
#4820 = CARTESIAN_POINT ( 'NONE',  ( 8.599030766203958009, -59.21224831720011395, 1.832439066039629916 ) ) ;
#4821 = EDGE_CURVE ( 'NONE', #5130, #304, #6902, .T. ) ;
#4822 = ORIENTED_EDGE ( 'NONE', *, *, #4041, .F. ) ;
#4823 = CARTESIAN_POINT ( 'NONE',  ( 65.68066376434035192, -11.76402373953423819, 76.00162494909807265 ) ) ;
#4824 = DIRECTION ( 'NONE',  ( 0.8420378618367653223, 0.5394184268574524488, -0.000000000000000000 ) ) ;
#4825 = AXIS2_PLACEMENT_3D ( 'NONE', #8741, #9919, #12290 ) ;
#4826 = CARTESIAN_POINT ( 'NONE',  ( 13.86173033120691223, -68.61243380581731799, -3.657093847832751710 ) ) ;
#4827 = DIRECTION ( 'NONE',  ( 1.000000000000000000, 1.239088197126290570E-16, -0.000000000000000000 ) ) ;
#4828 = CARTESIAN_POINT ( 'NONE',  ( -12.14523415828296571, -9.827631355817223024, -57.50000000000012079 ) ) ;
#4829 = AXIS2_PLACEMENT_3D ( 'NONE', #2380, #9392, #10464 ) ;
#4830 = EDGE_LOOP ( 'NONE', ( #6439, #3846, #717, #747 ) ) ;
#4831 = ORIENTED_EDGE ( 'NONE', *, *, #4998, .T. ) ;
#4832 = AXIS2_PLACEMENT_3D ( 'NONE', #14650, #12421, #3960 ) ;
#4833 = CARTESIAN_POINT ( 'NONE',  ( 64.11356537587559501, -11.94785244090458498, 75.19766410831374515 ) ) ;
#4834 = VERTEX_POINT ( 'NONE', #8262 ) ;
#4835 = DIRECTION ( 'NONE',  ( 0.8746197071345571672, -0.4848096202550662981, 0.000000000000000000 ) ) ;
#4836 = ORIENTED_EDGE ( 'NONE', *, *, #14223, .F. ) ;
#4837 = CARTESIAN_POINT ( 'NONE',  ( 28.33202942550559555, -66.31583591551219570, 4.137138225905043321 ) ) ;
#4838 = CIRCLE ( 'NONE', #8070, 0.5000000000000008882 ) ;
#4839 = ORIENTED_EDGE ( 'NONE', *, *, #8668, .F. ) ;
#4840 =( GEOMETRIC_REPRESENTATION_CONTEXT ( 3 ) GLOBAL_UNCERTAINTY_ASSIGNED_CONTEXT ( ( #8579 ) ) GLOBAL_UNIT_ASSIGNED_CONTEXT ( ( #854, #9101, #11632 ) ) REPRESENTATION_CONTEXT ( 'NONE', 'WORKASPACE' ) );
#4841 = CARTESIAN_POINT ( 'NONE',  ( -16.99999999999998579, -2.249290599286303927, -57.50000000000012079 ) ) ;
#4842 = CARTESIAN_POINT ( 'NONE',  ( -16.99999999999998579, -2.249290599286303927, 33.00000000000012790 ) ) ;
#4843 = ORIENTED_EDGE ( 'NONE', *, *, #10333, .F. ) ;
#4844 = ADVANCED_FACE ( 'NONE', ( #3784 ), #15178, .F. ) ;
#4845 = AXIS2_PLACEMENT_3D ( 'NONE', #4017, #9882, #7722 ) ;
#4846 = FACE_BOUND ( 'NONE', #7455, .T. ) ;
#4847 = AXIS2_PLACEMENT_3D ( 'NONE', #7265, #1192, #10583 ) ;
#4848 = CARTESIAN_POINT ( 'NONE',  ( 70.04947142428893869, -3.389475778999904598, 72.64451403610593161 ) ) ;
#4849 = ORIENTED_EDGE ( 'NONE', *, *, #4, .F. ) ;
#4850 = DIRECTION ( 'NONE',  ( 1.000000000000000000, 0.000000000000000000, 0.000000000000000000 ) ) ;
#4851 = CARTESIAN_POINT ( 'NONE',  ( -8.982583014919022446, 1.839844381040865118, -47.50000000000012079 ) ) ;
#4852 = CIRCLE ( 'NONE', #8758, 2.500000000000002220 ) ;
#4853 = LINE ( 'NONE', #2471, #10902 ) ;
#4854 = ORIENTED_EDGE ( 'NONE', *, *, #6998, .T. ) ;
#4855 = CARTESIAN_POINT ( 'NONE',  ( -12.09280073291247781, 0.000000000000000000, 11.78977872328357357 ) ) ;
#4856 = AXIS2_PLACEMENT_3D ( 'NONE', #2110, #9126, #13810 ) ;
#4857 = AXIS2_PLACEMENT_3D ( 'NONE', #9120, #13806, #5511 ) ;
#4858 = EDGE_LOOP ( 'NONE', ( #2067, #9678, #9070, #1302 ) ) ;
#4859 = CARTESIAN_POINT ( 'NONE',  ( 27.55953187330915810, 0.000000000000000000, 33.00000000000012790 ) ) ;
#4860 = ORIENTED_EDGE ( 'NONE', *, *, #2083, .F. ) ;
#4861 = EDGE_CURVE ( 'NONE', #11986, #3440, #9116, .T. ) ;
#4862 = EDGE_CURVE ( 'NONE', #4043, #10980, #3983, .T. ) ;
#4863 = CARTESIAN_POINT ( 'NONE',  ( 41.00000000000000711, 0.000000000000000000, 0.000000000000000000 ) ) ;
#4864 = CARTESIAN_POINT ( 'NONE',  ( 105.5545870572953930, 15.25070940071369563, 13.14990448602692474 ) ) ;
#4865 = CARTESIAN_POINT ( 'NONE',  ( 27.95143033160315937, -67.83931925369923022, 3.638954064322518889 ) ) ;
#4866 = EDGE_CURVE ( 'NONE', #7624, #2373, #11117, .T. ) ;
#4867 = AXIS2_PLACEMENT_3D ( 'NONE', #142, #3598, #10759 ) ;
#4868 = DIRECTION ( 'NONE',  ( 0.000000000000000000, 0.000000000000000000, 1.000000000000000000 ) ) ;
#4869 = DIRECTION ( 'NONE',  ( -1.000000000000000000, 0.000000000000000000, 0.000000000000000000 ) ) ;
#4870 = CIRCLE ( 'NONE', #1423, 1.000000000000000888 ) ;
#4871 = AXIS2_PLACEMENT_3D ( 'NONE', #10126, #14812, #4262 ) ;
#4872 = CIRCLE ( 'NONE', #5111, 0.9999999999999978906 ) ;
#4873 = LINE ( 'NONE', #10876, #11009 ) ;
#4874 = CYLINDRICAL_SURFACE ( 'NONE', #1213, 5.000000000000000000 ) ;
#4875 = CARTESIAN_POINT ( 'NONE',  ( 32.11820540151424552, -53.25766581158782742, 2.419604383416593674 ) ) ;
#4876 = PLANE ( 'NONE',  #8109 ) ;
#4877 = VECTOR ( 'NONE', #10075, 1000.000000000000000 ) ;
#4878 = VERTEX_POINT ( 'NONE', #2403 ) ;
#4879 = DIRECTION ( 'NONE',  ( -0.000000000000000000, -0.000000000000000000, 1.000000000000000000 ) ) ;
#4880 = ORIENTED_EDGE ( 'NONE', *, *, #1759, .T. ) ;
#4881 = CARTESIAN_POINT ( 'NONE',  ( 62.00000000000001421, -2.249290599286311032, 38.50000000000012790 ) ) ;
#4882 = CARTESIAN_POINT ( 'NONE',  ( 58.00000000000000711, 23.25070940071368852, -33.00000000000012790 ) ) ;
#4883 = VECTOR ( 'NONE', #11807, 1000.000000000000000 ) ;
#4884 = ORIENTED_EDGE ( 'NONE', *, *, #2453, .F. ) ;
#4885 = EDGE_CURVE ( 'NONE', #587, #8236, #13105, .T. ) ;
#4886 = DIRECTION ( 'NONE',  ( -0.4848096202550659650, -0.8746197071345572782, -0.000000000000000000 ) ) ;
#4887 = FACE_OUTER_BOUND ( 'NONE', #6463, .T. ) ;
#4888 = CARTESIAN_POINT ( 'NONE',  ( 69.40811084813233833, -3.478390292315104659, 76.12692897370897072 ) ) ;
#4889 = DIRECTION ( 'NONE',  ( -0.000000000000000000, -0.000000000000000000, 1.000000000000000000 ) ) ;
#4890 = CARTESIAN_POINT ( 'NONE',  ( 0.000000000000000000, 21.75070940071369918, 33.00000000000012790 ) ) ;
#4891 = CARTESIAN_POINT ( 'NONE',  ( 84.72310019870096198, 29.52935533987996664, 33.00000000000014211 ) ) ;
#4892 = CARTESIAN_POINT ( 'NONE',  ( 33.57093241131959616, -55.78447712832138450, 2.622266312280598033 ) ) ;
#4893 = EDGE_LOOP ( 'NONE', ( #1372, #8177, #14989, #976 ) ) ;
#4894 = CARTESIAN_POINT ( 'NONE',  ( -30.00000000000000000, 23.95881716715930665, -32.99999999999982236 ) ) ;
#4895 = UNCERTAINTY_MEASURE_WITH_UNIT (LENGTH_MEASURE( 1.000000000000000082E-05 ), #14256, 'distance_accuracy_value', 'NONE');
#4896 = VERTEX_POINT ( 'NONE', #10793 ) ;
#4897 = EDGE_CURVE ( 'NONE', #3324, #11072, #3481, .T. ) ;
#4898 = DIRECTION ( 'NONE',  ( 0.000000000000000000, 0.000000000000000000, 1.000000000000000000 ) ) ;
#4899 = ORIENTED_EDGE ( 'NONE', *, *, #12571, .T. ) ;
#4900 = CARTESIAN_POINT ( 'NONE',  ( -28.95977857253358323, -8.587818791446787614, -48.00000000000012079 ) ) ;
#4901 = CARTESIAN_POINT ( 'NONE',  ( 58.00000000000000711, -2.249290599286309256, 82.40005259842790508 ) ) ;
#4902 = AXIS2_PLACEMENT_3D ( 'NONE', #3489, #4641, #14031 ) ;
#4903 = DIRECTION ( 'NONE',  ( 0.000000000000000000, 1.000000000000000000, -0.000000000000000000 ) ) ;
#4904 = ORIENTED_EDGE ( 'NONE', *, *, #12171, .T. ) ;
#4905 = CARTESIAN_POINT ( 'NONE',  ( 8.126138517945966200, -57.16036077483330047, 1.814506011345170755 ) ) ;
#4906 = EDGE_CURVE ( 'NONE', #490, #2898, #5799, .T. ) ;
#4907 = ADVANCED_FACE ( 'NONE', ( #23 ), #9412, .T. ) ;
#4908 = CARTESIAN_POINT ( 'NONE',  ( -65.00000000000001421, -85.27429059928628874, -19.99999999999999645 ) ) ;
#4909 = DIRECTION ( 'NONE',  ( -0.000000000000000000, 0.000000000000000000, -1.000000000000000000 ) ) ;
#4910 = VECTOR ( 'NONE', #2853, 1000.000000000000000 ) ;
#4911 = EDGE_LOOP ( 'NONE', ( #15173, #5766, #7027, #12143 ) ) ;
#4912 = ORIENTED_EDGE ( 'NONE', *, *, #5007, .F. ) ;
#4913 = CARTESIAN_POINT ( 'NONE',  ( 80.00000000000001421, -85.24929059928629727, -8.000000000000001776 ) ) ;
#4914 = ORIENTED_EDGE ( 'NONE', *, *, #7117, .T. ) ;
#4915 = ADVANCED_FACE ( 'NONE', ( #4066 ), #9941, .F. ) ;
#4916 = CARTESIAN_POINT ( 'NONE',  ( -16.99999999999998579, 2.256146146571129218, 36.00000000000012079 ) ) ;
#4917 = ORIENTED_EDGE ( 'NONE', *, *, #5015, .T. ) ;
#4918 = DIRECTION ( 'NONE',  ( 0.000000000000000000, 0.000000000000000000, 1.000000000000000000 ) ) ;
#4919 = ORIENTED_EDGE ( 'NONE', *, *, #386, .F. ) ;
#4920 = DIRECTION ( 'NONE',  ( 1.000000000000000000, 1.156482317317870492E-16, 0.000000000000000000 ) ) ;
#4921 = DIRECTION ( 'NONE',  ( 0.000000000000000000, -1.000000000000000000, 0.000000000000000000 ) ) ;
#4922 = ORIENTED_EDGE ( 'NONE', *, *, #13204, .T. ) ;
#4923 = EDGE_CURVE ( 'NONE', #4512, #6172, #14408, .T. ) ;
#4924 = AXIS2_PLACEMENT_3D ( 'NONE', #3935, #14707, #6265 ) ;
#4925 = CARTESIAN_POINT ( 'NONE',  ( 105.5545870572953930, 23.25070940071369563, 13.14990448602693007 ) ) ;
#4926 = DIRECTION ( 'NONE',  ( 0.000000000000000000, 0.000000000000000000, 1.000000000000000000 ) ) ;
#4927 = VERTEX_POINT ( 'NONE', #328 ) ;
#4928 = CARTESIAN_POINT ( 'NONE',  ( 18.03113812440135888, 0.000000000000000000, 4.472107801411127959 ) ) ;
#4929 = LINE ( 'NONE', #2550, #12824 ) ;
#4930 = DIRECTION ( 'NONE',  ( 0.6293203910575899673, 0.7771459614506929237, 0.000000000000000000 ) ) ;
#4931 = ORIENTED_EDGE ( 'NONE', *, *, #9975, .F. ) ;
#4932 = CARTESIAN_POINT ( 'NONE',  ( 65.46435777888771668, -11.83269322980322968, 72.53932447423565577 ) ) ;
#4933 = EDGE_CURVE ( 'NONE', #60, #6843, #6937, .T. ) ;
#4934 = AXIS2_PLACEMENT_3D ( 'NONE', #12600, #7982, #2051 ) ;
#4935 = ORIENTED_EDGE ( 'NONE', *, *, #9516, .F. ) ;
#4936 = CARTESIAN_POINT ( 'NONE',  ( -80.00000000000001421, -72.24929059928631148, -34.99999999999999289 ) ) ;
#4937 = CARTESIAN_POINT ( 'NONE',  ( 65.00000000000001421, -85.24929059928629727, -19.99999999999999645 ) ) ;
#4938 = EDGE_LOOP ( 'NONE', ( #14440, #8595, #749, #10706 ) ) ;
#4939 = PRODUCT_CONTEXT ( 'NONE', #92, 'mechanical' ) ;
#4940 = DIRECTION ( 'NONE',  ( 0.000000000000000000, -0.000000000000000000, -1.000000000000000000 ) ) ;
#4941 = CARTESIAN_POINT ( 'NONE',  ( 31.13618595441765180, -61.88944072237682548, 2.366779157396534661 ) ) ;
#4942 = CARTESIAN_POINT ( 'NONE',  ( 21.74884261173415467, -82.24929059928629727, -6.000000000000000888 ) ) ;
#4943 = VECTOR ( 'NONE', #12300, 1000.000000000000000 ) ;
#4944 = CARTESIAN_POINT ( 'NONE',  ( 112.9262740340969060, 0.000000000000000000, 139.1143251403882459 ) ) ;
#4945 = CARTESIAN_POINT ( 'NONE',  ( 50.01091543003727224, 21.75070940071325865, 33.00000000000012790 ) ) ;
#4946 = DIRECTION ( 'NONE',  ( -0.8208219420614781825, 0.4549890321264266069, 0.3453061251629932493 ) ) ;
#4947 = CARTESIAN_POINT ( 'NONE',  ( 30.59878209274603478, -52.42197922347948946, 2.858153496903512725 ) ) ;
#4948 = CARTESIAN_POINT ( 'NONE',  ( 29.70251902843241965, -52.24929059928630437, -4.175384597093456662 ) ) ;
#4949 = VECTOR ( 'NONE', #14665, 1000.000000000000000 ) ;
#4950 = EDGE_CURVE ( 'NONE', #5064, #5118, #1778, .T. ) ;
#4951 = ADVANCED_FACE ( 'NONE', ( #2845 ), #608, .F. ) ;
#4952 = AXIS2_PLACEMENT_3D ( 'NONE', #12648, #6955, #5806 ) ;
#4953 = AXIS2_PLACEMENT_3D ( 'NONE', #6169, #9714, #11922 ) ;
#4954 = DIRECTION ( 'NONE',  ( -0.000000000000000000, -0.000000000000000000, -1.000000000000000000 ) ) ;
#4955 = EDGE_LOOP ( 'NONE', ( #12864, #9914, #10689, #8198 ) ) ;
#4956 = FACE_OUTER_BOUND ( 'NONE', #10380, .T. ) ;
#4957 = DIRECTION ( 'NONE',  ( 0.8746197071345571672, -0.4848096202550661871, 0.000000000000000000 ) ) ;
#4958 =( NAMED_UNIT ( * ) SI_UNIT ( $, .STERADIAN. ) SOLID_ANGLE_UNIT ( ) );
#4959 = DIRECTION ( 'NONE',  ( 1.000000000000000000, 0.000000000000000000, 0.000000000000000000 ) ) ;
#4960 = CARTESIAN_POINT ( 'NONE',  ( -65.00000000000001421, -85.27429059928630295, 19.99999999999999645 ) ) ;
#4961 = CIRCLE ( 'NONE', #13550, 4.000000000000003553 ) ;
#4962 = DIRECTION ( 'NONE',  ( 1.000000000000000000, -9.251858538542971581E-17, 0.000000000000000000 ) ) ;
#4963 = AXIS2_PLACEMENT_3D ( 'NONE', #10144, #14988, #13674 ) ;
#4964 = VECTOR ( 'NONE', #8207, 1000.000000000000000 ) ;
#4965 = CARTESIAN_POINT ( 'NONE',  ( 66.10060683232276801, -11.60666214070378111, 72.22272846899819854 ) ) ;
#4966 = DIRECTION ( 'NONE',  ( -0.8746197071345573892, 0.4848096202550659650, 0.000000000000000000 ) ) ;
#4967 = EDGE_CURVE ( 'NONE', #1918, #3601, #12349, .T. ) ;
#4968 = CARTESIAN_POINT ( 'NONE',  ( 31.45480550940234821, -52.78690463904968055, 2.615816816689916724 ) ) ;
#4969 = ORIENTED_EDGE ( 'NONE', *, *, #1143, .T. ) ;
#4970 = CARTESIAN_POINT ( 'NONE',  ( 61.36510378087922390, 1.530577915148011225, 60.61639468829817190 ) ) ;
#4971 = AXIS2_PLACEMENT_3D ( 'NONE', #12092, #12163, #1620 ) ;
#4972 = AXIS2_PLACEMENT_3D ( 'NONE', #119, #7113, #1340 ) ;
#4973 = ORIENTED_EDGE ( 'NONE', *, *, #9436, .F. ) ;
#4974 = DIRECTION ( 'NONE',  ( 1.000000000000000000, 0.000000000000000000, 0.000000000000000000 ) ) ;
#4975 = AXIS2_PLACEMENT_3D ( 'NONE', #15027, #7949, #9254 ) ;
#4976 = VERTEX_POINT ( 'NONE', #4146 ) ;
#4977 = ORIENTED_EDGE ( 'NONE', *, *, #11614, .F. ) ;
#4978 = CARTESIAN_POINT ( 'NONE',  ( 64.79775953413574996, -11.48183855866792058, 76.80558578852820517 ) ) ;
#4979 = DIRECTION ( 'NONE',  ( 0.000000000000000000, 0.000000000000000000, -1.000000000000000000 ) ) ;
#4980 = CARTESIAN_POINT ( 'NONE',  ( -21.66581936427349575, -2.249290599286304371, -57.50000000000012079 ) ) ;
#4981 = EDGE_LOOP ( 'NONE', ( #9685, #10145, #6681, #8940 ) ) ;
#4982 = VECTOR ( 'NONE', #12387, 1000.000000000000000 ) ;
#4983 = ORIENTED_EDGE ( 'NONE', *, *, #2019, .F. ) ;
#4984 = CIRCLE ( 'NONE', #13574, 6.484807146443463566 ) ;
#4985 = CARTESIAN_POINT ( 'NONE',  ( 23.36173033120691400, -82.24929059928629727, -6.000000000000000888 ) ) ;
#4986 = DIRECTION ( 'NONE',  ( -0.000000000000000000, -0.000000000000000000, 1.000000000000000000 ) ) ;
#4987 = CIRCLE ( 'NONE', #3021, 0.9999999999999954481 ) ;
#4988 = ORIENTED_EDGE ( 'NONE', *, *, #9193, .T. ) ;
#4989 = ORIENTED_EDGE ( 'NONE', *, *, #13743, .F. ) ;
#4990 = CARTESIAN_POINT ( 'NONE',  ( 64.46078417747735045, -11.72191032465318195, 76.42234406089987431 ) ) ;
#4991 = EDGE_CURVE ( 'NONE', #3132, #11072, #12848, .T. ) ;
#4992 = ORIENTED_EDGE ( 'NONE', *, *, #11137, .T. ) ;
#4993 = CARTESIAN_POINT ( 'NONE',  ( 9.412906046440658869, -59.69871785856275892, -2.790504257380244546 ) ) ;
#4994 = VERTEX_POINT ( 'NONE', #13466 ) ;
#4995 = CARTESIAN_POINT ( 'NONE',  ( 65.00000000000001421, -87.24929059928631148, 17.50000000000000000 ) ) ;
#4996 = ORIENTED_EDGE ( 'NONE', *, *, #9151, .F. ) ;
#4997 = EDGE_CURVE ( 'NONE', #2975, #1446, #5240, .T. ) ;
#4998 = EDGE_CURVE ( 'NONE', #12642, #2887, #3928, .T. ) ;
#4999 = AXIS2_PLACEMENT_3D ( 'NONE', #8231, #3371, #3531 ) ;
#5000 = FACE_OUTER_BOUND ( 'NONE', #1000, .T. ) ;
#5001 = CYLINDRICAL_SURFACE ( 'NONE', #4738, 0.4999999999999996114 ) ;
#5002 = ORIENTED_EDGE ( 'NONE', *, *, #9519, .T. ) ;
#5003 = CIRCLE ( 'NONE', #13587, 3.694885682587998765 ) ;
#5004 = CARTESIAN_POINT ( 'NONE',  ( 29.24282639220472291, -63.10178406536538631, -3.876738539648747928 ) ) ;
#5005 = CARTESIAN_POINT ( 'NONE',  ( -80.00000000000001421, -85.24929059928631148, -6.000000000000001776 ) ) ;
#5006 = ORIENTED_EDGE ( 'NONE', *, *, #9720, .F. ) ;
#5007 = EDGE_CURVE ( 'NONE', #5832, #9444, #5310, .T. ) ;
#5008 = FACE_OUTER_BOUND ( 'NONE', #14284, .T. ) ;
#5009 = DIRECTION ( 'NONE',  ( -0.2475627213817241101, 0.9688718692283695422, 0.000000000000000000 ) ) ;
#5010 = DIRECTION ( 'NONE',  ( -0.000000000000000000, 1.000000000000000000, 1.445602896647339163E-16 ) ) ;
#5011 = ORIENTED_EDGE ( 'NONE', *, *, #11614, .T. ) ;
#5012 = VECTOR ( 'NONE', #14132, 1000.000000000000000 ) ;
#5013 = DIRECTION ( 'NONE',  ( -1.000000000000000000, 0.000000000000000000, 0.000000000000000000 ) ) ;
#5014 = VECTOR ( 'NONE', #12158, 1000.000000000000000 ) ;
#5015 = EDGE_CURVE ( 'NONE', #5487, #10906, #3999, .T. ) ;
#5016 = VERTEX_POINT ( 'NONE', #10949 ) ;
#5017 = DIRECTION ( 'NONE',  ( -0.000000000000000000, -0.000000000000000000, -1.000000000000000000 ) ) ;
#5018 = ORIENTED_EDGE ( 'NONE', *, *, #1123, .F. ) ;
#5019 = ADVANCED_FACE ( 'NONE', ( #7323 ), #12313, .T. ) ;
#5020 = ITEM_DEFINED_TRANSFORMATION ( 'NONE', 'NONE', #9775,  #6315 ) ;
#5021 = DIRECTION ( 'NONE',  ( 0.8208219420614786266, -0.4549890321264269399, -0.3453061251629919171 ) ) ;
#5022 = LINE ( 'NONE', #1624, #7435 ) ;
#5023 = CARTESIAN_POINT ( 'NONE',  ( -8.650962968042231083, 2.291620771759304898, -48.06291368403883268 ) ) ;
#5024 = CARTESIAN_POINT ( 'NONE',  ( 17.36157654472070888, -73.69234276600499811, 6.062089035220985522 ) ) ;
#5025 = EDGE_CURVE ( 'NONE', #2895, #1585, #7480, .T. ) ;
#5026 = CARTESIAN_POINT ( 'NONE',  ( 33.12442989620986822, -59.21224831720011395, 1.832439066039631914 ) ) ;
#5027 = CARTESIAN_POINT ( 'NONE',  ( 109.8334623555409735, 0.000000000000000000, 139.1143251403882459 ) ) ;
#5028 = CARTESIAN_POINT ( 'NONE',  ( -9.345472082723105700, -7.632075232572700152, -48.02161282446750334 ) ) ;
#5029 = LINE ( 'NONE', #337, #13342 ) ;
#5030 = CARTESIAN_POINT ( 'NONE',  ( 32.69777265694848722, -53.84505747417108523, -3.062469901903030589 ) ) ;
#5031 = CARTESIAN_POINT ( 'NONE',  ( -21.85476584171713199, 5.329050157244537900, 57.50000000000012079 ) ) ;
#5032 = VERTEX_POINT ( 'NONE', #1478 ) ;
#5033 = DIRECTION ( 'NONE',  ( 0.000000000000000000, 0.000000000000000000, 1.000000000000000000 ) ) ;
#5034 = CARTESIAN_POINT ( 'NONE',  ( 80.18290120114222930, 23.25070940071369208, 84.20452624982236500 ) ) ;
#5035 = EDGE_CURVE ( 'NONE', #5069, #9890, #6184, .T. ) ;
#5036 = CARTESIAN_POINT ( 'NONE',  ( 73.69809405469877106, 25.52935533987996664, -21.00807340887166674 ) ) ;
#5037 = CARTESIAN_POINT ( 'NONE',  ( 69.97972559771834256, -3.172990592780090324, 75.33564424702136364 ) ) ;
#5038 = CARTESIAN_POINT ( 'NONE',  ( 64.20414115715628611, -11.89030131877283480, 72.55252335815228548 ) ) ;
#5039 = EDGE_CURVE ( 'NONE', #2280, #12222, #5022, .T. ) ;
#5040 = EDGE_CURVE ( 'NONE', #3737, #14173, #9726, .T. ) ;
#5041 = CARTESIAN_POINT ( 'NONE',  ( 27.33382790127957662, -69.39711819508849544, -4.502057496415715399 ) ) ;
#5042 = PLANE ( 'NONE',  #7411 ) ;
#5043 = ORIENTED_EDGE ( 'NONE', *, *, #9837, .F. ) ;
#5044 = LINE ( 'NONE', #5986, #7058 ) ;
#5045 = UNCERTAINTY_MEASURE_WITH_UNIT (LENGTH_MEASURE( 1.000000000000000082E-05 ), #13903, 'distance_accuracy_value', 'NONE');
#5046 = VERTEX_POINT ( 'NONE', #8555 ) ;
#5047 = DIRECTION ( 'NONE',  ( 0.000000000000000000, -1.000000000000000000, 0.000000000000000000 ) ) ;
#5048 = ORIENTED_EDGE ( 'NONE', *, *, #5612, .F. ) ;
#5049 = ORIENTED_EDGE ( 'NONE', *, *, #5859, .T. ) ;
#5051 = ORIENTED_EDGE ( 'NONE', *, *, #3303, .T. ) ;
#5050 = CARTESIAN_POINT ( 'NONE',  ( -9.345472082723105700, -7.632075232572700152, 48.02161282446750334 ) ) ;
#5052 = FACE_OUTER_BOUND ( 'NONE', #713, .T. ) ;
#5053 = EDGE_CURVE ( 'NONE', #3249, #12316, #8697, .T. ) ;
#5054 = EDGE_CURVE ( 'NONE', #5462, #4285, #1556, .T. ) ;
#5055 = FACE_OUTER_BOUND ( 'NONE', #186, .T. ) ;
#5056 = PRODUCT_DEFINITION ( 'UNKNOWN', '', #5854, #9363 ) ;
#5057 = ORIENTED_EDGE ( 'NONE', *, *, #6340, .F. ) ;
#5058 = CARTESIAN_POINT ( 'NONE',  ( 8.782543352270323567, -56.07132046089833466, 2.830553478268754031 ) ) ;
#5059 = FACE_OUTER_BOUND ( 'NONE', #14115, .T. ) ;
#5060 = DIRECTION ( 'NONE',  ( -1.000000000000000000, -0.000000000000000000, -0.000000000000000000 ) ) ;
#5061 = VERTEX_POINT ( 'NONE', #14767 ) ;
#5062 = CARTESIAN_POINT ( 'NONE',  ( 65.61547001893620745, -10.82016271803256657, 77.19766410831377357 ) ) ;
#5063 = VERTEX_POINT ( 'NONE', #11227 ) ;
#5064 = VERTEX_POINT ( 'NONE', #4295 ) ;
#5065 = CARTESIAN_POINT ( 'NONE',  ( 80.00000000000001421, -76.24929059928631148, 6.000000000000000000 ) ) ;
#5066 = ORIENTED_EDGE ( 'NONE', *, *, #1823, .F. ) ;
#5067 = CARTESIAN_POINT ( 'NONE',  ( 28.79421079956515683, -63.81378734511702788, 4.043274055230560826 ) ) ;
#5068 = VECTOR ( 'NONE', #13927, 1000.000000000000000 ) ;
#5069 = VERTEX_POINT ( 'NONE', #2071 ) ;
#5070 = DIRECTION ( 'NONE',  ( 0.000000000000000000, -0.000000000000000000, -1.000000000000000000 ) ) ;
#5071 = CARTESIAN_POINT ( 'NONE',  ( 20.86173033120691045, -57.24929059928630437, -3.000000000000000888 ) ) ;
#5072 = ORIENTED_EDGE ( 'NONE', *, *, #11516, .F. ) ;
#5073 = CARTESIAN_POINT ( 'NONE',  ( 30.26140529968839843, -61.79747627231853357, -3.500139319475241262 ) ) ;
#5074 = PRODUCT_DEFINITION_SHAPE ( 'NONE', 'NONE',  #15228 ) ;
#5075 = ORIENTED_EDGE ( 'NONE', *, *, #14778, .T. ) ;
#5076 = CIRCLE ( 'NONE', #9758, 0.5000000000000004441 ) ;
#5077 = DIRECTION ( 'NONE',  ( 0.000000000000000000, 1.000000000000000000, -0.000000000000000000 ) ) ;
#5078 = CARTESIAN_POINT ( 'NONE',  ( 48.00000000000000000, -2.664535259100377906E-14, -33.00000000000012790 ) ) ;
#5079 = LINE ( 'NONE', #14471, #14346 ) ;
#5080 = ORIENTED_EDGE ( 'NONE', *, *, #2292, .F. ) ;
#5081 = CARTESIAN_POINT ( 'NONE',  ( -24.66543232906180805, 3.122884019241207287, 48.02064173568555816 ) ) ;
#5083 = ORIENTED_EDGE ( 'NONE', *, *, #4041, .T. ) ;
#5082 = ADVANCED_FACE ( 'NONE', ( #9238 ), #6274, .F. ) ;
#5084 = EDGE_CURVE ( 'NONE', #4409, #8448, #4984, .T. ) ;
#5085 = ORIENTED_EDGE ( 'NONE', *, *, #7153, .F. ) ;
#5086 = PLANE ( 'NONE',  #2775 ) ;
#5087 = EDGE_CURVE ( 'NONE', #2887, #3754, #13770, .T. ) ;
#5088 = EDGE_LOOP ( 'NONE', ( #2964, #14634, #9945, #10176 ) ) ;
#5089 = AXIS2_PLACEMENT_3D ( 'NONE', #5915, #2591, #12050 ) ;
#5090 = SHAPE_DEFINITION_REPRESENTATION ( #12617, #10411 ) ;
#5091 = CARTESIAN_POINT ( 'NONE',  ( 76.14589960879430919, -7.734310727912411920, 75.19766410831374515 ) ) ;
#5092 = DIRECTION ( 'NONE',  ( -0.000000000000000000, 0.000000000000000000, 1.000000000000000000 ) ) ;
#5093 = LINE ( 'NONE', #13389, #8004 ) ;
#5094 = ORIENTED_EDGE ( 'NONE', *, *, #13338, .T. ) ;
#5095 = CARTESIAN_POINT ( 'NONE',  ( 12.57704357998833089, -50.05591495609738217, 4.211963358982736771 ) ) ;
#5096 = AXIS2_PLACEMENT_3D ( 'NONE', #2661, #2585, #10742 ) ;
#5097 = DIRECTION ( 'NONE',  ( 1.000000000000000000, 0.000000000000000000, 0.000000000000000000 ) ) ;
#5098 = DIRECTION ( 'NONE',  ( 0.000000000000000000, 0.000000000000000000, 1.000000000000000000 ) ) ;
#5099 = EDGE_CURVE ( 'NONE', #14376, #4084, #12624, .T. ) ;
#5100 = CARTESIAN_POINT ( 'NONE',  ( 32.23959774372725207, -53.36427686165168893, 2.382617577203031800 ) ) ;
#5101 = DIRECTION ( 'NONE',  ( 0.000000000000000000, -0.000000000000000000, -1.000000000000000000 ) ) ;
#5102 = ADVANCED_FACE ( 'NONE', ( #7773 ), #12461, .F. ) ;
#5103 = AXIS2_PLACEMENT_3D ( 'NONE', #121, #4807, #268 ) ;
#5104 = CARTESIAN_POINT ( 'NONE',  ( -8.679783256197868724, 2.339454207888506776, 48.10016682092218332 ) ) ;
#5105 = ORIENTED_EDGE ( 'NONE', *, *, #9436, .T. ) ;
#5106 = SURFACE_SIDE_STYLE ('',( #551 ) ) ;
#5107 = PLANE ( 'NONE',  #1463 ) ;
#5108 = CIRCLE ( 'NONE', #10514, 31.00000000000000000 ) ;
#5109 = CARTESIAN_POINT ( 'NONE',  ( 9.211295467215947497, 29.36814620404575038, 73.19766410831374515 ) ) ;
#5110 = CIRCLE ( 'NONE', #7078, 4.000000000000003553 ) ;
#5111 = AXIS2_PLACEMENT_3D ( 'NONE', #8943, #3170, #2088 ) ;
#5112 = CARTESIAN_POINT ( 'NONE',  ( -33.07225206673494711, -1.856991049495498425, 57.50000000000012079 ) ) ;
#5113 = LINE ( 'NONE', #14276, #7916 ) ;
#5114 = FACE_OUTER_BOUND ( 'NONE', #5541, .T. ) ;
#5115 = CARTESIAN_POINT ( 'NONE',  ( -24.80190065418678458, -6.760980545838084943, -48.43121057161747700 ) ) ;
#5116 = VECTOR ( 'NONE', #13998, 1000.000000000000000 ) ;
#5117 = VECTOR ( 'NONE', #6785, 1000.000000000000000 ) ;
#5118 = VERTEX_POINT ( 'NONE', #5468 ) ;
#5119 = CARTESIAN_POINT ( 'NONE',  ( 34.22806330994987434, -51.17708206442508612, -2.732753929480980837 ) ) ;
#5120 = EDGE_LOOP ( 'NONE', ( #5219, #14772 ) ) ;
#5121 = EDGE_CURVE ( 'NONE', #8955, #7944, #9076, .T. ) ;
#5122 = ORIENTED_EDGE ( 'NONE', *, *, #7446, .F. ) ;
#5123 = LINE ( 'NONE', #9825, #9641 ) ;
#5124 = CARTESIAN_POINT ( 'NONE',  ( 0.000000000000000000, 21.75070940071322667, 139.1143251403882459 ) ) ;
#5125 = ORIENTED_EDGE ( 'NONE', *, *, #12152, .T. ) ;
#5126 = VERTEX_POINT ( 'NONE', #4380 ) ;
#5127 = CARTESIAN_POINT ( 'NONE',  ( 88.00000000000000000, 23.25070940071369208, 33.00000000000014211 ) ) ;
#5128 = CARTESIAN_POINT ( 'NONE',  ( -26.99999999999998224, -69.24929059928631148, -32.99999999999999289 ) ) ;
#5129 = DIRECTION ( 'NONE',  ( 0.000000000000000000, 0.000000000000000000, -1.000000000000000000 ) ) ;
#5130 = VERTEX_POINT ( 'NONE', #12544 ) ;
#5131 = DIRECTION ( 'NONE',  ( -0.8746197071345572782, 0.4848096202550659650, -0.000000000000000000 ) ) ;
#5132 = CARTESIAN_POINT ( 'NONE',  ( -65.00000000000001421, -87.24929059928631148, -19.99999999999999645 ) ) ;
#5133 = DIRECTION ( 'NONE',  ( 1.000000000000000000, -0.000000000000000000, 0.000000000000000000 ) ) ;
#5134 = ORIENTED_EDGE ( 'NONE', *, *, #12608, .F. ) ;
#5135 = CARTESIAN_POINT ( 'NONE',  ( -12.09280073291247426, -82.24929059928629727, -11.78977872328358067 ) ) ;
#5136 = EDGE_CURVE ( 'NONE', #6626, #4096, #6759, .T. ) ;
#5137 = ORIENTED_EDGE ( 'NONE', *, *, #12365, .T. ) ;
#5138 = CARTESIAN_POINT ( 'NONE',  ( 80.00000000000001421, -85.24929059928629727, 8.000000000000001776 ) ) ;
#5139 = ORIENTED_EDGE ( 'NONE', *, *, #9322, .F. ) ;
#5140 = CARTESIAN_POINT ( 'NONE',  ( 28.60124718008176359, -65.57050171853848042, 4.044987206835600091 ) ) ;
#5141 = VERTEX_POINT ( 'NONE', #11376 ) ;
#5142 = CYLINDRICAL_SURFACE ( 'NONE', #9764, 1.000000000000007550 ) ;
#5143 = DIRECTION ( 'NONE',  ( 0.000000000000000000, 0.000000000000000000, 1.000000000000000000 ) ) ;
#5144 = ORIENTED_EDGE ( 'NONE', *, *, #5665, .T. ) ;
#5145 = CARTESIAN_POINT ( 'NONE',  ( 27.94158133900257113, -67.90279320104600913, -3.641642753169207936 ) ) ;
#5146 = ORIENTED_EDGE ( 'NONE', *, *, #2957, .F. ) ;
#5147 = AXIS2_PLACEMENT_3D ( 'NONE', #11177, #861, #11553 ) ;
#5148 = AXIS2_PLACEMENT_3D ( 'NONE', #3167, #5405, #3245 ) ;
#5149 = DIRECTION ( 'NONE',  ( -0.5006040828730773384, 0.8656763553492754504, 0.000000000000000000 ) ) ;
#5150 = CARTESIAN_POINT ( 'NONE',  ( 58.00000000000000711, -2.249290599286311032, 33.00000000000012790 ) ) ;
#5151 = B_SPLINE_CURVE_WITH_KNOTS ( 'NONE', 3,
 ( #4007, #11165, #8932, #6696, #2936, #13623, #5478, #11085, #10168, #7781 ),
 .UNSPECIFIED., .F., .F.,
 ( 4, 2, 2, 2, 4 ),
 ( 0.000000000000000000, 0.0003835113287520873016, 0.0007670226575041746032, 0.001150533986256262013, 0.001534045315008349206 ),
 .UNSPECIFIED. ) ;
#5152 = DIRECTION ( 'NONE',  ( 0.000000000000000000, 1.000000000000000000, -0.000000000000000000 ) ) ;
#5153 = EDGE_LOOP ( 'NONE', ( #603, #5509, #5997, #2264 ) ) ;
#5154 = ADVANCED_FACE ( 'NONE', ( #12390, #834 ), #3226, .F. ) ;
#5155 = LINE ( 'NONE', #6095, #10281 ) ;
#5156 = ORIENTED_EDGE ( 'NONE', *, *, #3068, .F. ) ;
#5157 = ORIENTED_EDGE ( 'NONE', *, *, #2651, .F. ) ;
#5158 = APPLICATION_CONTEXT ( 'automotive_design' ) ;
#5159 = EDGE_LOOP ( 'NONE', ( #979, #8993, #2751, #12606 ) ) ;
#5160 = PLANE ( 'NONE',  #4971 ) ;
#5161 = VECTOR ( 'NONE', #9662, 1000.000000000000000 ) ;
#5162 = APPLICATION_PROTOCOL_DEFINITION ( 'draft international standard', 'automotive_design', 1998, #6727 ) ;
#5163 = CARTESIAN_POINT ( 'NONE',  ( 58.00000000000000711, -6.754727345143743733, 38.00000000000012079 ) ) ;
#5164 = CARTESIAN_POINT ( 'NONE',  ( -2.016677571526633510E-15, 23.25070940071368497, 33.00000000000012790 ) ) ;
#5165 = LINE ( 'NONE', #9870, #11938 ) ;
#5166 = ADVANCED_FACE ( 'NONE', ( #13850 ), #3305, .F. ) ;
#5167 = CARTESIAN_POINT ( 'NONE',  ( 96.00000000000002842, 2.750709400713692965, 33.00000000000012790 ) ) ;
#5168 = PLANE ( 'NONE',  #11044 ) ;
#5169 = CARTESIAN_POINT ( 'NONE',  ( -5.290523468902621929, 4.522075770548486418, -57.50000000000012079 ) ) ;
#5170 = CARTESIAN_POINT ( 'NONE',  ( 13.65275068252246449, -65.32322779889733511, -4.310009693574635925 ) ) ;
#5171 = ADVANCED_FACE ( 'NONE', ( #11612 ), #3462, .T. ) ;
#5172 = ORIENTED_EDGE ( 'NONE', *, *, #7417, .T. ) ;
#5173 = DIRECTION ( 'NONE',  ( -1.000000000000000000, -0.000000000000000000, -0.000000000000000000 ) ) ;
#5174 = DIRECTION ( 'NONE',  ( -0.3020115420618247892, 0.1674077314120183957, -0.9384901064608620613 ) ) ;
#5175 = CARTESIAN_POINT ( 'NONE',  ( 58.00000000000000711, -2.249290599286309256, 82.40005259842790508 ) ) ;
#5176 = B_SPLINE_CURVE_WITH_KNOTS ( 'NONE', 3,
 ( #9066, #1976, #6750, #9155 ),
 .UNSPECIFIED., .F., .F.,
 ( 4, 4 ),
 ( 0.000000000000000000, 0.001771943201165730340 ),
 .UNSPECIFIED. ) ;
#5177 = ADVANCED_FACE ( 'NONE', ( #3383 ), #4615, .F. ) ;
#5178 = EDGE_CURVE ( 'NONE', #9615, #153, #7229, .T. ) ;
#5179 = DIRECTION ( 'NONE',  ( 0.2135987722749887463, 0.9769214730379394140, 0.000000000000000000 ) ) ;
#5180 = EDGE_CURVE ( 'NONE', #3352, #3629, #11689, .T. ) ;
#5181 = DIRECTION ( 'NONE',  ( 0.000000000000000000, 0.000000000000000000, 1.000000000000000000 ) ) ;
#5182 = CIRCLE ( 'NONE', #11818, 4.505436745857433145 ) ;
#5183 = CARTESIAN_POINT ( 'NONE',  ( 27.81150698810987265, -69.39711819508849544, -3.980554831151301265 ) ) ;
#5184 =( BOUNDED_SURFACE ( )  B_SPLINE_SURFACE ( 3, 2, ( 
 ( #9335, #14026, #8187 ),
 ( #8341, #3561, #8266 ),
 ( #9493, #12956, #12890 ),
 ( #2407, #1247, #5958 ),
 ( #3640, #7022, #11868 ),
 ( #4480, #9187, #13952 ) ),
 .UNSPECIFIED., .F., .F., .F. ) 
 B_SPLINE_SURFACE_WITH_KNOTS ( ( 4, 2, 4 ),
 ( 3, 3 ),
 ( -6.505213034913026604E-18, 0.001008510999900119739, 0.002017021999800245984 ),
 ( 0.000000000000000000, 1.000000000000000000 ),
 .UNSPECIFIED. ) 
 GEOMETRIC_REPRESENTATION_ITEM ( )  RATIONAL_B_SPLINE_SURFACE ( (
 ( 1.000000000000000000, 0.8053615646146046192, 1.000000000000000000),
 ( 1.000000000000000000, 0.8146689552414230207, 1.000000000000000000),
 ( 1.000000000000000000, 0.8215765256475128231, 1.000000000000000000),
 ( 1.000000000000000000, 0.8301698670438529826, 1.000000000000000000),
 ( 1.000000000000000000, 0.8316880482410894393, 1.000000000000000000),
 ( 1.000000000000000000, 0.8308543624379411963, 1.000000000000000000) ) ) 
 REPRESENTATION_ITEM ( '' )  SURFACE ( )  );
#5185 = ADVANCED_FACE ( 'NONE', ( #1301 ), #7001, .T. ) ;
#5186 = CARTESIAN_POINT ( 'NONE',  ( 29.24198010098109890, -64.22824823034754615, -3.135769320951036221 ) ) ;
#5187 = VECTOR ( 'NONE', #11066, 1000.000000000000114 ) ;
#5188 = ORIENTED_EDGE ( 'NONE', *, *, #974, .T. ) ;
#5189 = CARTESIAN_POINT ( 'NONE',  ( 46.91810375148135392, 21.75070940071322667, 33.00000000000012790 ) ) ;
#5190 = EDGE_LOOP ( 'NONE', ( #5273, #9054, #5684, #8894, #13312, #12148 ) ) ;
#5191 = CARTESIAN_POINT ( 'NONE',  ( 46.91810375148135392, 23.25070940071368852, -33.00000000000012790 ) ) ;
#5192 = CARTESIAN_POINT ( 'NONE',  ( 56.59738969056744651, 0.000000000000000000, 33.00000000000012790 ) ) ;
#5193 = ORIENTED_EDGE ( 'NONE', *, *, #10022, .T. ) ;
#5194 = CIRCLE ( 'NONE', #2499, 0.4999999999999995559 ) ;
#5195 = DIRECTION ( 'NONE',  ( 0.000000000000000000, 0.000000000000000000, 1.000000000000000000 ) ) ;
#5196 = CARTESIAN_POINT ( 'NONE',  ( 0.000000000000000000, 0.000000000000000000, -33.00000000000012790 ) ) ;
#5197 = ORIENTED_EDGE ( 'NONE', *, *, #4132, .T. ) ;
#5198 = CIRCLE ( 'NONE', #2504, 0.7892041907098253928 ) ;
#5199 = EDGE_CURVE ( 'NONE', #13187, #927, #5863, .T. ) ;
#5200 = CARTESIAN_POINT ( 'NONE',  ( -21.16581936427349575, -2.249290599286304371, -50.50000000000012079 ) ) ;
#5201 = CARTESIAN_POINT ( 'NONE',  ( -30.00000000000000000, -74.24929059928631148, -32.99999999999999289 ) ) ;
#5202 = DIRECTION ( 'NONE',  ( -0.000000000000000000, 1.000000000000000000, 1.445602896647339163E-16 ) ) ;
#5203 = AXIS2_PLACEMENT_3D ( 'NONE', #10560, #12797, #2241 ) ;
#5204 = VECTOR ( 'NONE', #15089, 1000.000000000000000 ) ;
#5205 = DIRECTION ( 'NONE',  ( -0.9744556954135545901, -0.2245798247307308204, 0.000000000000000000 ) ) ;
#5206 = ORIENTED_EDGE ( 'NONE', *, *, #409, .T. ) ;
#5207 = AXIS2_PLACEMENT_3D ( 'NONE', #5707, #12626, #4384 ) ;
#5208 = ORIENTED_EDGE ( 'NONE', *, *, #13504, .F. ) ;
#5209 = PLANE ( 'NONE',  #14912 ) ;
#5210 = EDGE_LOOP ( 'NONE', ( #3817, #5925, #12985, #8662 ) ) ;
#5211 = CARTESIAN_POINT ( 'NONE',  ( 29.69047892279255407, -53.28399145779480506, -4.141535524925019196 ) ) ;
#5212 = ORIENTED_EDGE ( 'NONE', *, *, #11700, .T. ) ;
#5213 = DIRECTION ( 'NONE',  ( -1.000000000000000000, 0.000000000000000000, 0.000000000000000000 ) ) ;
#5214 = DIRECTION ( 'NONE',  ( 1.000000000000000000, 8.673617379884027583E-16, 0.000000000000000000 ) ) ;
#5215 = EDGE_LOOP ( 'NONE', ( #12306, #13549, #10979, #7371 ) ) ;
#5216 = VECTOR ( 'NONE', #5835, 999.9999999999998863 ) ;
#5217 = CARTESIAN_POINT ( 'NONE',  ( 65.13162939602317181, -11.91918766459985157, 73.19766410831374515 ) ) ;
#5218 = CARTESIAN_POINT ( 'NONE',  ( 64.90552635791956959, 22.43695620243006772, -33.00000000000012790 ) ) ;
#5219 = ORIENTED_EDGE ( 'NONE', *, *, #11873, .F. ) ;
#5220 = AXIS2_PLACEMENT_3D ( 'NONE', #8074, #4532, #9307 ) ;
#5221 = VECTOR ( 'NONE', #12720, 1000.000000000000000 ) ;
#5222 = CARTESIAN_POINT ( 'NONE',  ( 30.84433510184662097, -61.22098757969241944, -3.286659897588250612 ) ) ;
#5223 = ORIENTED_EDGE ( 'NONE', *, *, #14223, .T. ) ;
#5224 = ADVANCED_FACE ( 'NONE', ( #6082 ), #2227, .T. ) ;
#5225 = EDGE_CURVE ( 'NONE', #13804, #8896, #2462, .T. ) ;
#5226 = AXIS2_PLACEMENT_3D ( 'NONE', #12781, #10465, #14005 ) ;
#5227 = CYLINDRICAL_SURFACE ( 'NONE', #8540, 0.7892041907098262810 ) ;
#5228 = DIRECTION ( 'NONE',  ( 0.000000000000000000, 0.000000000000000000, -1.000000000000000000 ) ) ;
#5229 = LINE ( 'NONE', #9859, #5758 ) ;
#5230 = EDGE_LOOP ( 'NONE', ( #7380, #7053, #5072, #5849 ) ) ;
#5231 = PLANE ( 'NONE',  #13467 ) ;
#5232 = EDGE_LOOP ( 'NONE', ( #8647, #5473, #4214, #726 ) ) ;
#5233 = PRODUCT_DEFINITION_SHAPE ( 'NONE', 'NONE',  #10316 ) ;
#5234 = VERTEX_POINT ( 'NONE', #11842 ) ;
#5235 = CIRCLE ( 'NONE', #13834, 2.499999999999995115 ) ;
#5236 = ORIENTED_EDGE ( 'NONE', *, *, #13202, .T. ) ;
#5237 = AXIS2_PLACEMENT_3D ( 'NONE', #2852, #4071, #4154 ) ;
#5238 = PRESENTATION_STYLE_ASSIGNMENT (( #10445 ) ) ;
#5239 = DIRECTION ( 'NONE',  ( 1.000000000000000000, 0.000000000000000000, 0.000000000000000000 ) ) ;
#5240 = LINE ( 'NONE', #5164, #14792 ) ;
#5241 = EDGE_CURVE ( 'NONE', #2361, #2895, #15157, .T. ) ;
#5242 = PLANE ( 'NONE',  #8272 ) ;
#5243 = ADVANCED_FACE ( 'NONE', ( #12863 ), #6014, .F. ) ;
#5244 = ORIENTED_EDGE ( 'NONE', *, *, #9422, .T. ) ;
#5245 = EDGE_CURVE ( 'NONE', #10926, #981, #3289, .T. ) ;
#5246 = CIRCLE ( 'NONE', #566, 2.500000000000002220 ) ;
#5247 = DIRECTION ( 'NONE',  ( -0.000000000000000000, 0.000000000000000000, -1.000000000000000000 ) ) ;
#5248 = DIRECTION ( 'NONE',  ( -0.000000000000000000, 1.000000000000000000, 1.445602896647339163E-16 ) ) ;
#5249 = AXIS2_PLACEMENT_3D ( 'NONE', #9246, #4701, #2391 ) ;
#5250 = CARTESIAN_POINT ( 'NONE',  ( 12.36791015745245836, -52.24929059928631148, 3.199931146564429341 ) ) ;
#5251 = LINE ( 'NONE', #3161, #1471 ) ;
#5252 = VERTEX_POINT ( 'NONE', #8080 ) ;
#5253 = CARTESIAN_POINT ( 'NONE',  ( 69.46221311437309964, -2.886128739015261679, 73.19766410831374515 ) ) ;
#5254 = B_SPLINE_CURVE_WITH_KNOTS ( 'NONE', 3,
 ( #11260, #4180, #3045, #13418, #2882, #7580, #716, #5423 ),
 .UNSPECIFIED., .F., .F.,
 ( 4, 2, 2, 4 ),
 ( 0.000000000000000000, 0.0002685324218445791621, 0.0005370648436891570232, 0.001074129687378310794 ),
 .UNSPECIFIED. ) ;
#5255 = CARTESIAN_POINT ( 'NONE',  ( -9.209612907684750382, 2.258800220783480750, 47.62582736825572738 ) ) ;
#5256 = ORIENTED_EDGE ( 'NONE', *, *, #12312, .T. ) ;
#5257 = CARTESIAN_POINT ( 'NONE',  ( 52.83848824477699679, -4.298675648159541396, 54.56811043785582882 ) ) ;
#5258 = CARTESIAN_POINT ( 'NONE',  ( -80.00000000000001421, -72.24929059928631148, 32.99999999999999289 ) ) ;
#5259 = CARTESIAN_POINT ( 'NONE',  ( 29.35555050496136431, -52.24929059928631148, -3.199931146564432449 ) ) ;
#5260 = FACE_OUTER_BOUND ( 'NONE', #115, .T. ) ;
#5261 = ORIENTED_EDGE ( 'NONE', *, *, #13873, .T. ) ;
#5262 = CARTESIAN_POINT ( 'NONE',  ( 124.7888489864508728, -33.55418379006125917, 51.74171249506144932 ) ) ;
#5263 = ORIENTED_EDGE ( 'NONE', *, *, #2779, .F. ) ;
#5264 = EDGE_CURVE ( 'NONE', #10195, #12779, #6450, .T. ) ;
#5265 = CARTESIAN_POINT ( 'NONE',  ( 53.45023817967523172, -5.433760736713491468, 60.61639468829817190 ) ) ;
#5266 = DIRECTION ( 'NONE',  ( 0.8746197071345569451, -0.4848096202550666312, 0.000000000000000000 ) ) ;
#5267 = CARTESIAN_POINT ( 'NONE',  ( 84.72310019870096198, 29.52935533987996664, 33.00000000000014211 ) ) ;
#5268 = ORIENTED_EDGE ( 'NONE', *, *, #11010, .F. ) ;
#5269 = CARTESIAN_POINT ( 'NONE',  ( 28.25575485889338978, -61.89598878741227139, -4.173736770051541534 ) ) ;
#5270 = ORIENTED_EDGE ( 'NONE', *, *, #4866, .F. ) ;
#5271 = LINE ( 'NONE', #6279, #520 ) ;
#5272 = DIRECTION ( 'NONE',  ( 1.000000000000000000, 0.000000000000000000, 0.000000000000000000 ) ) ;
#5273 = ORIENTED_EDGE ( 'NONE', *, *, #9971, .T. ) ;
#5275 = ORIENTED_EDGE ( 'NONE', *, *, #10456, .T. ) ;
#5274 = PLANE ( 'NONE',  #8663 ) ;
#5276 = DIRECTION ( 'NONE',  ( 1.000000000000000000, 0.000000000000000000, 0.000000000000000000 ) ) ;
#5277 = ADVANCED_FACE ( 'NONE', ( #2309 ), #1892, .T. ) ;
#5278 = EDGE_CURVE ( 'NONE', #1911, #2542, #15060, .T. ) ;
#5279 = DIRECTION ( 'NONE',  ( -0.8420378618367644341, -0.5394184268574535590, -0.000000000000000000 ) ) ;
#5280 = CARTESIAN_POINT ( 'NONE',  ( 12.36791015745246547, -52.24929059928630437, 3.199931146564424456 ) ) ;
#5281 = DIRECTION ( 'NONE',  ( -0.000000000000000000, 0.000000000000000000, 1.000000000000000000 ) ) ;
#5282 = DIRECTION ( 'NONE',  ( -0.000000000000000000, -0.000000000000000000, 1.000000000000000000 ) ) ;
#5283 = EDGE_CURVE ( 'NONE', #12099, #11185, #11769, .T. ) ;
#5284 = ORIENTED_EDGE ( 'NONE', *, *, #1968, .F. ) ;
#5285 = ADVANCED_FACE ( 'NONE', ( #4774 ), #13374, .T. ) ;
#5286 = CARTESIAN_POINT ( 'NONE',  ( 20.86173033120691045, -53.24929059928630437, 0.000000000000000000 ) ) ;
#5287 = ORIENTED_EDGE ( 'NONE', *, *, #9975, .T. ) ;
#5288 = EDGE_LOOP ( 'NONE', ( #940, #8878, #1056, #1336 ) ) ;
#5289 = DIRECTION ( 'NONE',  ( 0.000000000000000000, 0.000000000000000000, 1.000000000000000000 ) ) ;
#5290 = VERTEX_POINT ( 'NONE', #8679 ) ;
#5291 = CARTESIAN_POINT ( 'NONE',  ( -8.509932750408504276, 13.28409490805591808, 57.50000000000012079 ) ) ;
#5292 = DIRECTION ( 'NONE',  ( -0.000000000000000000, -0.000000000000000000, -1.000000000000000000 ) ) ;
#5293 = PLANE ( 'NONE',  #9992 ) ;
#5294 = CARTESIAN_POINT ( 'NONE',  ( -12.83418063572647760, -2.249290599286303927, -50.00000000000012079 ) ) ;
#5295 = ORIENTED_EDGE ( 'NONE', *, *, #12463, .T. ) ;
#5296 = CARTESIAN_POINT ( 'NONE',  ( 29.65531183511549074, -63.62021712492606440, -2.966460067271383672 ) ) ;
#5297 = ORIENTED_EDGE ( 'NONE', *, *, #1759, .F. ) ;
#5298 = CLOSED_SHELL ( 'NONE', ( #2279, #8838, #205, #2310, #158, #989, #295, #14342, #4726, #9925, #6833, #5770, #3240, #10021, #8792, #4218, #9347, #11590, #466, #841, #10171, #11159, #2355, #5808, #13395, #8012, #1329, #4951, #6597, #4844, #595, #13870, #1407, #14473, #19, #4612, #10820, #8389, #4033, #9757, #7954, #11082 ) ) ;
#5299 = FACE_OUTER_BOUND ( 'NONE', #10332, .T. ) ;
#5300 = CARTESIAN_POINT ( 'NONE',  ( 3.703153296433914665, -69.39711819508849544, 2.500000000000000000 ) ) ;
#5301 = LINE ( 'NONE', #1614, #3039 ) ;
#5302 = ORIENTED_EDGE ( 'NONE', *, *, #10466, .F. ) ;
#5303 = AXIS2_PLACEMENT_3D ( 'NONE', #12888, #11637, #11316 ) ;
#5304 = CARTESIAN_POINT ( 'NONE',  ( 56.59738969056744651, 23.25070940071368852, -33.00000000000012790 ) ) ;
#5305 = EDGE_LOOP ( 'NONE', ( #683, #11068, #14117, #5938 ) ) ;
#5306 = ORIENTED_EDGE ( 'NONE', *, *, #292, .T. ) ;
#5307 = EDGE_LOOP ( 'NONE', ( #15136, #9084, #13494, #12709 ) ) ;
#5308 = EDGE_CURVE ( 'NONE', #13577, #12159, #2684, .T. ) ;
#5309 = LINE ( 'NONE', #10007, #14212 ) ;
#5310 = LINE ( 'NONE', #11017, #6686 ) ;
#5311 = EDGE_CURVE ( 'NONE', #1096, #14996, #1536, .T. ) ;
#5312 = CARTESIAN_POINT ( 'NONE',  ( -10.08762850755046969, -8.023634329963208245, -47.66527511103321046 ) ) ;
#5313 = VECTOR ( 'NONE', #8095, 1000.000000000000000 ) ;
#5314 = ORIENTED_EDGE ( 'NONE', *, *, #503, .F. ) ;
#5315 = CARTESIAN_POINT ( 'NONE',  ( -8.754378065084850391, 2.456381933588792865, -48.23869654929341522 ) ) ;
#5316 = CARTESIAN_POINT ( 'NONE',  ( 65.61367503392970946, -11.78584904878405304, 72.43470407172173964 ) ) ;
#5317 = DIRECTION ( 'NONE',  ( 0.000000000000000000, 0.000000000000000000, -1.000000000000000000 ) ) ;
#5318 = CARTESIAN_POINT ( 'NONE',  ( -16.99999999999998579, -2.249290599286303927, 58.00000000000012079 ) ) ;
#5319 = CARTESIAN_POINT ( 'NONE',  ( 13.00536048170743797, -65.29678988936899486, -3.348867343500126825 ) ) ;
#5320 = VERTEX_POINT ( 'NONE', #8744 ) ;
#5321 = EDGE_LOOP ( 'NONE', ( #10858, #9774, #1602, #5841 ) ) ;
#5322 = CARTESIAN_POINT ( 'NONE',  ( 33.63308522438084935, -56.83262086368724653, 1.823905708653747348 ) ) ;
#5323 = B_SPLINE_CURVE_WITH_KNOTS ( 'NONE', 3,
 ( #258, #6034, #7255, #10719, #14262, #1249, #7105, #5804, #2412, #9495, #11792, #10572, #5961, #1331 ),
 .UNSPECIFIED., .F., .F.,
 ( 4, 2, 2, 2, 2, 2, 4 ),
 ( 0.000000000000000000, 0.002515995007885566369, 0.003773992511828368635, 0.005031990015771170902, 0.006289987519713973602, 0.007547985023656774567, 0.01006398003154241119 ),
 .UNSPECIFIED. ) ;
#5324 = AXIS2_PLACEMENT_3D ( 'NONE', #6141, #2519, #10752 ) ;
#5325 = DIRECTION ( 'NONE',  ( -0.000000000000000000, -0.000000000000000000, 1.000000000000000000 ) ) ;
#5326 = EDGE_CURVE ( 'NONE', #750, #4627, #6374, .T. ) ;
#5327 = VERTEX_POINT ( 'NONE', #2830 ) ;
#5328 = EDGE_CURVE ( 'NONE', #14748, #8583, #9935, .T. ) ;
#5329 = CARTESIAN_POINT ( 'NONE',  ( 9.074525391310594102, -58.48797006926988473, -2.754379914540418639 ) ) ;
#5330 = ORIENTED_EDGE ( 'NONE', *, *, #9364, .F. ) ;
#5331 = CIRCLE ( 'NONE', #5096, 0.4999999999999999445 ) ;
#5332 = DIRECTION ( 'NONE',  ( -0.000000000000000000, -0.000000000000000000, -1.000000000000000000 ) ) ;
#5333 = AXIS2_PLACEMENT_3D ( 'NONE', #1343, #7037, #8503 ) ;
#5334 = CARTESIAN_POINT ( 'NONE',  ( 27.41385764376421363, -69.39711819508850965, -4.459166325353804083 ) ) ;
#5335 = CARTESIAN_POINT ( 'NONE',  ( -2.016677571526633510E-15, 23.25070940071368497, 139.1143251403882459 ) ) ;
#5336 = CARTESIAN_POINT ( 'NONE',  ( -24.96483633670257873, -6.441926561070030033, -48.01692658285762150 ) ) ;
#5337 = ORIENTED_EDGE ( 'NONE', *, *, #4469, .F. ) ;
#5338 = ORIENTED_EDGE ( 'NONE', *, *, #6398, .F. ) ;
#5339 = ADVANCED_FACE ( 'NONE', ( #8604 ), #7526, .F. ) ;
#5340 = CARTESIAN_POINT ( 'NONE',  ( 32.59856662516318693, -59.08346394664149415, -2.725125706471997145 ) ) ;
#5341 = VECTOR ( 'NONE', #11655, 1000.000000000000000 ) ;
#5342 = EDGE_LOOP ( 'NONE', ( #296, #12667 ) ) ;
#5343 = FACE_OUTER_BOUND ( 'NONE', #8038, .T. ) ;
#5344 = DIRECTION ( 'NONE',  ( -0.8746197071345569451, 0.4848096202550666312, 0.000000000000000000 ) ) ;
#5345 = AXIS2_PLACEMENT_3D ( 'NONE', #9331, #15177, #393 ) ;
#5346 = EDGE_LOOP ( 'NONE', ( #13604, #961, #3865, #12162, #10595, #12330, #8973, #674, #2835, #8549, #9880 ) ) ;
#5347 = DIRECTION ( 'NONE',  ( -0.000000000000000000, -0.000000000000000000, 1.000000000000000000 ) ) ;
#5348 = FACE_OUTER_BOUND ( 'NONE', #4955, .T. ) ;
#5349 = ORIENTED_EDGE ( 'NONE', *, *, #2323, .T. ) ;
#5350 = CARTESIAN_POINT ( 'NONE',  ( 8.599030766203958009, -59.21224831720011395, -1.832439066039622144 ) ) ;
#5351 = CARTESIAN_POINT ( 'NONE',  ( 12.03298173962126860, -53.28399145779480506, 4.141535524925031631 ) ) ;
#5352 = CARTESIAN_POINT ( 'NONE',  ( 67.21328690825531282, 25.52935533987996664, -33.00000000000012790 ) ) ;
#5353 = CLOSED_SHELL ( 'NONE', ( #3849, #14515, #11108, #13304, #7733, #4779, #837, #2287, #5224, #799, #14374, #9773, #3877, #9365, #14127, #5339, #3485, #14029, #8428, #14550, #845, #741, #1830, #1841, #33, #5102, #14027, #7427, #10278, #1053, #1261, #14091, #4269, #14660, #7192, #13655, #8208, #9382, #14360, #13876, #1153, #11806, #10012, #7714, #8569, #3507, #9719, #8216, #14782, #11305, #15163, #12659, #5177, #9796, #12964, #8575, #12774, #9284, #4014, #15025, #11388, #11371, #4819, #14310, #10934, #6432, #8528, #2352, #4520, #9033, #2216, #11460, #11862, #7344, #751, #1280, #573, #5166, #3390, #4335, #3776, #5823, #3259 ) ) ;
#5354 = PRODUCT ( 'MAS-317', 'MAS-317', '', ( #7321 ) ) ;
#5355 = TOROIDAL_SURFACE ( 'NONE', #12740, 8.500000000000000000, 0.5000000000000000000 ) ;
#5356 = CARTESIAN_POINT ( 'NONE',  ( 118.0000000000000284, 23.25070940071369563, 139.1143251403882459 ) ) ;
#5357 = CARTESIAN_POINT ( 'NONE',  ( 67.21328690825529861, 29.52935533987996664, 21.00807340887166674 ) ) ;
#5358 = ADVANCED_FACE ( 'NONE', ( #9777 ), #5001, .T. ) ;
#5359 = EDGE_LOOP ( 'NONE', ( #7356, #5636, #13280, #10495 ) ) ;
#5360 = DIRECTION ( 'NONE',  ( -0.000000000000000000, 1.000000000000000000, 1.445602896647339163E-16 ) ) ;
#5361 = EDGE_LOOP ( 'NONE', ( #5066, #5956, #5919, #7313 ) ) ;
#5362 = DIRECTION ( 'NONE',  ( 0.000000000000000000, 0.000000000000000000, 1.000000000000000000 ) ) ;
#5363 = AXIS2_PLACEMENT_3D ( 'NONE', #7692, #7537, #11071 ) ;
#5364 = ORIENTED_EDGE ( 'NONE', *, *, #1789, .F. ) ;
#5365 = CARTESIAN_POINT ( 'NONE',  ( -12.41494337171168283, -9.406612424898836977, -58.00000000000012079 ) ) ;
#5366 = PLANE ( 'NONE',  #4825 ) ;
#5367 = AXIS2_PLACEMENT_3D ( 'NONE', #3389, #2152, #7935 ) ;
#5368 = DIRECTION ( 'NONE',  ( 1.000000000000000000, 0.000000000000000000, 0.000000000000000000 ) ) ;
#5369 = DIRECTION ( 'NONE',  ( -1.000000000000000000, -8.673617379884035472E-17, 0.000000000000000000 ) ) ;
#5370 = EDGE_LOOP ( 'NONE', ( #13066, #10462, #7377, #1882, #15009, #2810, #7162 ) ) ;
#5371 = EDGE_CURVE ( 'NONE', #9847, #13591, #11140, .T. ) ;
#5372 = ADVANCED_FACE ( 'NONE', ( #14390 ), #7196, .T. ) ;
#5373 = DIRECTION ( 'NONE',  ( 0.000000000000000000, 0.000000000000000000, -1.000000000000000000 ) ) ;
#5374 = ORIENTED_EDGE ( 'NONE', *, *, #9815, .T. ) ;
#5375 = DIRECTION ( 'NONE',  ( 0.000000000000000000, 0.000000000000000000, -1.000000000000000000 ) ) ;
#5376 = LINE ( 'NONE', #7839, #95 ) ;
#5377 = CARTESIAN_POINT ( 'NONE',  ( -3.035218482312739496, 5.248692456477230373, 57.50000000000012079 ) ) ;
#5378 = EDGE_CURVE ( 'NONE', #10204, #14789, #12632, .T. ) ;
#5379 = ORIENTED_EDGE ( 'NONE', *, *, #8061, .T. ) ;
#5380 = LINE ( 'NONE', #7766, #2900 ) ;
#5381 = CIRCLE ( 'NONE', #229, 0.5000000000000000000 ) ;
#5382 = VERTEX_POINT ( 'NONE', #1606 ) ;
#5383 = VERTEX_POINT ( 'NONE', #13444 ) ;
#5384 = EDGE_LOOP ( 'NONE', ( #1467, #10823, #4533, #9827 ) ) ;
#5385 = LINE ( 'NONE', #12309, #6442 ) ;
#5386 = ITEM_DEFINED_TRANSFORMATION ( 'NONE', 'NONE', #11726,  #6315 ) ;
#5387 = DIRECTION ( 'NONE',  ( 0.000000000000000000, 0.000000000000000000, -1.000000000000000000 ) ) ;
#5388 = CARTESIAN_POINT ( 'NONE',  ( -24.38033816570045076, 2.914516366099690448, -47.90685900410169040 ) ) ;
#5389 = CIRCLE ( 'NONE', #2929, 0.5000000000000000000 ) ;
#5390 = CIRCLE ( 'NONE', #8096, 0.5000000000000004441 ) ;
#5391 = CARTESIAN_POINT ( 'NONE',  ( 103.2469880950108063, 0.000000000000000000, 33.00000000000012790 ) ) ;
#5392 = ORIENTED_EDGE ( 'NONE', *, *, #264, .F. ) ;
#5393 = CARTESIAN_POINT ( 'NONE',  ( -16.99999999999998579, -2.249290599286303927, 58.00000000000012079 ) ) ;
#5394 = DIRECTION ( 'NONE',  ( -0.8746197071345576113, 0.4848096202550652434, 0.000000000000000000 ) ) ;
#5395 = EDGE_CURVE ( 'NONE', #8222, #3759, #548, .T. ) ;
#5396 = CARTESIAN_POINT ( 'NONE',  ( 118.5627027169299765, -35.81974489651393156, 54.40673322733726280 ) ) ;
#5397 = CARTESIAN_POINT ( 'NONE',  ( 12.48063427020827021, -63.10178406536854112, -3.876738539648207471 ) ) ;
#5398 = VERTEX_POINT ( 'NONE', #6444 ) ;
#5399 = LINE ( 'NONE', #9091, #11750 ) ;
#5400 = VECTOR ( 'NONE', #8066, 1000.000000000000000 ) ;
#5401 = CIRCLE ( 'NONE', #1950, 5.496540510819668768 ) ;
#5402 = CARTESIAN_POINT ( 'NONE',  ( -9.097850607046364502, 2.059891325575069043, 47.52616914649232172 ) ) ;
#5403 = EDGE_LOOP ( 'NONE', ( #11144, #3949, #357, #6231 ) ) ;
#5404 = LINE ( 'NONE', #7015, #7913 ) ;
#5405 = DIRECTION ( 'NONE',  ( -0.000000000000000000, -0.000000000000000000, -1.000000000000000000 ) ) ;
#5406 = DIRECTION ( 'NONE',  ( 0.000000000000000000, 0.000000000000000000, 1.000000000000000000 ) ) ;
#5407 = LINE ( 'NONE', #12563, #5221 ) ;
#5408 = ORIENTED_EDGE ( 'NONE', *, *, #4559, .F. ) ;
#5409 = DIRECTION ( 'NONE',  ( 0.000000000000000000, 0.000000000000000000, 1.000000000000000000 ) ) ;
#5410 = AXIS2_PLACEMENT_3D ( 'NONE', #732, #590, #13668 ) ;
#5411 = EDGE_CURVE ( 'NONE', #13900, #10942, #8538, .T. ) ;
#5412 = CARTESIAN_POINT ( 'NONE',  ( 55.36337191871069763, -7.136966431295542534, 48.51982618741349285 ) ) ;
#5413 = EDGE_CURVE ( 'NONE', #8760, #11327, #453, .T. ) ;
#5414 = CARTESIAN_POINT ( 'NONE',  ( -24.80875755767168300, -6.748058119754043460, -48.36238429206898815 ) ) ;
#5415 = VERTEX_POINT ( 'NONE', #1682 ) ;
#5416 = CARTESIAN_POINT ( 'NONE',  ( 23.47466359740176145, -53.10810670090258867, -6.494041865157049287 ) ) ;
#5417 = ORIENTED_EDGE ( 'NONE', *, *, #5917, .F. ) ;
#5418 = DIRECTION ( 'NONE',  ( -0.8656763553492639041, -0.5006040828730973224, -0.000000000000000000 ) ) ;
#5419 = CARTESIAN_POINT ( 'NONE',  ( 11.26881178693570362, -52.38369591842261030, 2.898182089495347391 ) ) ;
#5420 = VECTOR ( 'NONE', #11400, 1000.000000000000000 ) ;
#5421 = EDGE_LOOP ( 'NONE', ( #12419, #9390, #7577, #1238 ) ) ;
#5422 = CARTESIAN_POINT ( 'NONE',  ( 58.00000000000000711, 23.25070940071368852, 33.00000000000012790 ) ) ;
#5423 = CARTESIAN_POINT ( 'NONE',  ( 14.38963276113425138, -69.39711819508849544, -4.502057496415714510 ) ) ;
#5424 = VERTEX_POINT ( 'NONE', #2907 ) ;
#5425 = CARTESIAN_POINT ( 'NONE',  ( 10.00023835250150483, -61.42570632716525125, -2.132522520905374197 ) ) ;
#5426 = EDGE_CURVE ( 'NONE', #11056, #12155, #6709, .T. ) ;
#5427 = VECTOR ( 'NONE', #3275, 1000.000000000000000 ) ;
#5428 = EDGE_CURVE ( 'NONE', #2922, #12406, #8215, .T. ) ;
#5429 = CARTESIAN_POINT ( 'NONE',  ( 30.65234355186507997, 21.75070940071312364, 33.00000000000012790 ) ) ;
#5430 = CYLINDRICAL_SURFACE ( 'NONE', #4871, 31.00000000000000000 ) ;
#5431 = CARTESIAN_POINT ( 'NONE',  ( 80.00000000000001421, -74.24929059928631148, 32.99999999999999289 ) ) ;
#5432 = DIRECTION ( 'NONE',  ( -1.000000000000000000, 6.938893903907228378E-17, 0.000000000000000000 ) ) ;
#5433 = CARTESIAN_POINT ( 'NONE',  ( -25.24562193491511763, -6.954963132161501527, -48.23869654929341522 ) ) ;
#5434 = EDGE_LOOP ( 'NONE', ( #2992, #12627, #6836, #9824 ) ) ;
#5435 = DIRECTION ( 'NONE',  ( 1.224646799147353207E-16, 1.000000000000000000, -0.000000000000000000 ) ) ;
#5436 = AXIS2_PLACEMENT_3D ( 'NONE', #1219, #14081, #1293 ) ;
#5437 = VERTEX_POINT ( 'NONE', #6822 ) ;
#5438 = CARTESIAN_POINT ( 'NONE',  ( 32.51083376785603463, -54.90380519981211194, -3.064473585392911481 ) ) ;
#5439 = ORIENTED_EDGE ( 'NONE', *, *, #2036, .T. ) ;
#5440 = DIRECTION ( 'NONE',  ( -0.000000000000000000, 0.000000000000000000, -1.000000000000000000 ) ) ;
#5441 = VECTOR ( 'NONE', #1465, 1000.000000000000000 ) ;
#5442 = CIRCLE ( 'NONE', #3961, 2.524999999999999467 ) ;
#5443 = FACE_OUTER_BOUND ( 'NONE', #10242, .T. ) ;
#5444 = LINE ( 'NONE', #8904, #7290 ) ;
#5445 = LINE ( 'NONE', #10142, #784 ) ;
#5446 = VERTEX_POINT ( 'NONE', #7908 ) ;
#5447 = CARTESIAN_POINT ( 'NONE',  ( 58.99998260679605266, 10.75660737539945622, 84.20452624982236500 ) ) ;
#5448 = CIRCLE ( 'NONE', #7421, 3.999999999999999112 ) ;
#5449 = EDGE_LOOP ( 'NONE', ( #12886, #1728, #12499, #3291 ) ) ;
#5450 = AXIS2_PLACEMENT_3D ( 'NONE', #5124, #8877, #8721 ) ;
#5451 = COLOUR_RGB ( '',0.7921568627450980005, 0.8196078431372548767, 0.9333333333333333481 ) ;
#5452 = CARTESIAN_POINT ( 'NONE',  ( 65.35217890228821602, -11.86361580896913459, 75.75081418052154447 ) ) ;
#5453 = CARTESIAN_POINT ( 'NONE',  ( 9.668720703607657896, -54.31361072226496134, -3.260388240305699181 ) ) ;
#5454 = CARTESIAN_POINT ( 'NONE',  ( -30.00000000000000000, -74.24929059928631148, -32.99999999999999289 ) ) ;
#5455 = EDGE_CURVE ( 'NONE', #8958, #1506, #5603, .T. ) ;
#5456 = CARTESIAN_POINT ( 'NONE',  ( 57.83740799265796539, -7.800393779465814248, 60.61639468829817190 ) ) ;
#5457 = ORIENTED_EDGE ( 'NONE', *, *, #7541, .F. ) ;
#5458 = LINE ( 'NONE', #4605, #14943 ) ;
#5459 = EDGE_CURVE ( 'NONE', #12204, #404, #13672, .T. ) ;
#5460 = VERTEX_POINT ( 'NONE', #5294 ) ;
#5461 = CARTESIAN_POINT ( 'NONE',  ( -30.80945343098651890, -5.389243620311580329, 48.00000000000012079 ) ) ;
#5462 = VERTEX_POINT ( 'NONE', #735 ) ;
#5463 = EDGE_CURVE ( 'NONE', #14822, #2753, #9988, .T. ) ;
#5464 = ORIENTED_EDGE ( 'NONE', *, *, #1529, .T. ) ;
#5465 = CARTESIAN_POINT ( 'NONE',  ( 27.86173033120691045, -69.39711819508849544, 3.619682905202613377 ) ) ;
#5466 = VECTOR ( 'NONE', #6324, 1000.000000000000000 ) ;
#5467 = CARTESIAN_POINT ( 'NONE',  ( 9.400986902400736867, -59.70726391082678930, -2.784470044084383478 ) ) ;
#5468 = CARTESIAN_POINT ( 'NONE',  ( 70.26445833701072274, -4.474174595298148205, 72.19766410831374515 ) ) ;
#5469 = VECTOR ( 'NONE', #13302, 1000.000000000000000 ) ;
#5470 = EDGE_CURVE ( 'NONE', #11241, #3666, #10214, .T. ) ;
#5471 = ADVANCED_FACE ( 'NONE', ( #14671 ), #10296, .F. ) ;
#5472 = CARTESIAN_POINT ( 'NONE',  ( -3.190546569013415379, 0.8906624217387615339, -48.50000000000012079 ) ) ;
#5473 = ORIENTED_EDGE ( 'NONE', *, *, #3106, .F. ) ;
#5474 = DIRECTION ( 'NONE',  ( -0.000000000000000000, -0.000000000000000000, -1.000000000000000000 ) ) ;
#5475 = CARTESIAN_POINT ( 'NONE',  ( 69.97972559857380759, -3.172990593254279457, 75.35198908857846334 ) ) ;
#5476 = VECTOR ( 'NONE', #606, 1000.000000000000000 ) ;
#5477 = DIRECTION ( 'NONE',  ( 0.000000000000000000, 0.000000000000000000, -1.000000000000000000 ) ) ;
#5478 = CARTESIAN_POINT ( 'NONE',  ( -9.394882438906904554, 2.563636819302931524, 48.00656353678737531 ) ) ;
#5479 = CARTESIAN_POINT ( 'NONE',  ( 12.92924986285064115, -63.81378734511702788, -4.043274055231452557 ) ) ;
#5480 = EDGE_CURVE ( 'NONE', #10942, #12159, #70, .T. ) ;
#5481 = ORIENTED_EDGE ( 'NONE', *, *, #13730, .T. ) ;
#5482 = CARTESIAN_POINT ( 'NONE',  ( 33.55155325696184576, -55.68585955703496637, 1.912302604851222387 ) ) ;
#5483 = CIRCLE ( 'NONE', #3272, 0.7892041907098245046 ) ;
#5484 = EDGE_CURVE ( 'NONE', #4049, #7613, #4200, .T. ) ;
#5485 = EDGE_CURVE ( 'NONE', #6079, #3807, #4358, .T. ) ;
#5486 = DIRECTION ( 'NONE',  ( 0.000000000000000000, -0.000000000000000000, 1.000000000000000000 ) ) ;
#5487 = VERTEX_POINT ( 'NONE', #7754 ) ;
#5488 = CARTESIAN_POINT ( 'NONE',  ( 27.32685193182241079, -68.54636829475870741, -4.542647641079959442 ) ) ;
#5489 = DIRECTION ( 'NONE',  ( 1.156482317317870492E-16, -1.000000000000000000, 0.000000000000000000 ) ) ;
#5490 = DIRECTION ( 'NONE',  ( -0.000000000000000000, 0.000000000000000000, -1.000000000000000000 ) ) ;
#5491 = PLANE ( 'NONE',  #13564 ) ;
#5492 = ORIENTED_EDGE ( 'NONE', *, *, #5180, .T. ) ;
#5493 = CARTESIAN_POINT ( 'NONE',  ( -16.99999999999998579, -2.249290599286303927, -38.00000000000012079 ) ) ;
#5494 = AXIS2_PLACEMENT_3D ( 'NONE', #1975, #4135, #898 ) ;
#5495 = CIRCLE ( 'NONE', #7697, 4.000000000000003553 ) ;
#5496 = LINE ( 'NONE', #5644, #11247 ) ;
#5497 = CARTESIAN_POINT ( 'NONE',  ( 23.36173033120691400, -85.24929059928631148, -6.000000000000000888 ) ) ;
#5498 = CARTESIAN_POINT ( 'NONE',  ( 76.12673345701679750, -7.723686756500376838, 73.07464432123545350 ) ) ;
#5499 = CARTESIAN_POINT ( 'NONE',  ( -24.64572710697934710, -6.998028550906933098, -47.88483805351501132 ) ) ;
#5500 = ORIENTED_EDGE ( 'NONE', *, *, #4716, .F. ) ;
#5501 = ORIENTED_EDGE ( 'NONE', *, *, #11517, .F. ) ;
#5502 = FACE_OUTER_BOUND ( 'NONE', #13366, .T. ) ;
#5503 = VERTEX_POINT ( 'NONE', #8823 ) ;
#5504 = EDGE_CURVE ( 'NONE', #11327, #13149, #6514, .T. ) ;
#5505 = DIRECTION ( 'NONE',  ( -0.8124228799517130284, 0.5830686615922384686, 0.000000000000000000 ) ) ;
#5506 = CARTESIAN_POINT ( 'NONE',  ( 12.36791015745245836, -52.24929059928631148, 3.199931146564429341 ) ) ;
#5507 = VERTEX_POINT ( 'NONE', #9060 ) ;
#5508 = VECTOR ( 'NONE', #13922, 1000.000000000000000 ) ;
#5509 = ORIENTED_EDGE ( 'NONE', *, *, #13548, .T. ) ;
#5510 = CARTESIAN_POINT ( 'NONE',  ( 80.18290120114222930, 25.52935533987996664, -33.00000000000012790 ) ) ;
#5511 = DIRECTION ( 'NONE',  ( -1.000000000000000000, 0.000000000000000000, 0.000000000000000000 ) ) ;
#5512 = EDGE_CURVE ( 'NONE', #12689, #1978, #13829, .T. ) ;
#5513 = CARTESIAN_POINT ( 'NONE',  ( 13.50577566551452513, -66.70046270226335139, 4.174231074480405645 ) ) ;
#5514 = DIRECTION ( 'NONE',  ( 0.000000000000000000, 0.000000000000000000, 1.000000000000000000 ) ) ;
#5515 = CARTESIAN_POINT ( 'NONE',  ( 33.63091130056225353, -56.19153130592571443, -1.861773613859164511 ) ) ;
#5516 = CARTESIAN_POINT ( 'NONE',  ( 9.573486461617511267, -58.98766849246937483, 1.832439066040226106 ) ) ;
#5517 = FACE_OUTER_BOUND ( 'NONE', #6355, .T. ) ;
#5518 = LINE ( 'NONE', #10203, #10026 ) ;
#5519 = ORIENTED_EDGE ( 'NONE', *, *, #1084, .F. ) ;
#5520 = CARTESIAN_POINT ( 'NONE',  ( 13.88366620244440064, -68.65220048136326625, -4.053998922580050568 ) ) ;
#5521 = ORIENTED_EDGE ( 'NONE', *, *, #5704, .F. ) ;
#5522 = DIRECTION ( 'NONE',  ( 0.000000000000000000, 0.000000000000000000, 1.000000000000000000 ) ) ;
#5523 = VERTEX_POINT ( 'NONE', #11276 ) ;
#5524 = CARTESIAN_POINT ( 'NONE',  ( 27.40406279159242331, -67.79239290436652254, 4.531617596074583254 ) ) ;
#5525 = EDGE_CURVE ( 'NONE', #13907, #14067, #661, .T. ) ;
#5526 = ADVANCED_FACE ( 'NONE', ( #6665 ), #6744, .T. ) ;
#5527 = CARTESIAN_POINT ( 'NONE',  ( 69.46454297106444642, -2.294433322023680333, 73.19766410831374515 ) ) ;
#5528 = DIRECTION ( 'NONE',  ( 0.000000000000000000, 1.000000000000000000, 0.000000000000000000 ) ) ;
#5529 = DIRECTION ( 'NONE',  ( -0.000000000000000000, 1.734723475976817547E-15, 1.000000000000000000 ) ) ;
#5530 = CARTESIAN_POINT ( 'NONE',  ( 17.09549820959326638, -96.56299909827106376, -1.347403282660980084 ) ) ;
#5531 = ORIENTED_EDGE ( 'NONE', *, *, #3488, .F. ) ;
#5532 = CARTESIAN_POINT ( 'NONE',  ( 65.00000000000001421, -85.24929059928631148, 17.47499999999999787 ) ) ;
#5533 = CARTESIAN_POINT ( 'NONE',  ( 10.83605996619203715, -52.52081589074905565, -2.777424068826388925 ) ) ;
#5534 = CARTESIAN_POINT ( 'NONE',  ( 10.62011700622559474, -60.64100864355887666, -2.132522520905393737 ) ) ;
#5535 = DIRECTION ( 'NONE',  ( -0.000000000000000000, 0.000000000000000000, 1.000000000000000000 ) ) ;
#5536 = ORIENTED_EDGE ( 'NONE', *, *, #4183, .F. ) ;
#5537 = DIRECTION ( 'NONE',  ( 0.000000000000000000, -1.000000000000000000, 0.000000000000000000 ) ) ;
#5538 = ORIENTED_EDGE ( 'NONE', *, *, #5007, .T. ) ;
#5539 = DIRECTION ( 'NONE',  ( -1.000000000000000000, -8.673617379884035472E-17, 0.000000000000000000 ) ) ;
#5540 = ORIENTED_EDGE ( 'NONE', *, *, #1175, .T. ) ;
#5541 = EDGE_LOOP ( 'NONE', ( #9090, #422, #8691, #6135 ) ) ;
#5542 = DIRECTION ( 'NONE',  ( 1.000000000000000000, 3.565820478396769525E-15, 0.000000000000000000 ) ) ;
#5543 = CARTESIAN_POINT ( 'NONE',  ( 68.00000000000001421, 1.887379141862766624E-13, 33.00000000000012790 ) ) ;
#5544 = CARTESIAN_POINT ( 'NONE',  ( 12.03298173962126150, -53.28399145779480506, -4.141535524925039624 ) ) ;
#5545 = PRESENTATION_STYLE_ASSIGNMENT (( #3156 ) ) ;
#5546 = ORIENTED_EDGE ( 'NONE', *, *, #12, .T. ) ;
#5547 = CARTESIAN_POINT ( 'NONE',  ( -12.14523415828296216, -9.827631355817223024, 57.50000000000012079 ) ) ;
#5548 = DIRECTION ( 'NONE',  ( 1.000000000000000000, 0.000000000000000000, 0.000000000000000000 ) ) ;
#5549 = CARTESIAN_POINT ( 'NONE',  ( 32.97430361024782997, -56.32704560409237615, -2.799357392884137763 ) ) ;
#5550 = DIRECTION ( 'NONE',  ( 0.000000000000000000, 0.000000000000000000, 1.000000000000000000 ) ) ;
#5551 = CARTESIAN_POINT ( 'NONE',  ( 34.91116660049384279, -47.87980016383388460, 2.732839075344419388 ) ) ;
#5552 = EDGE_LOOP ( 'NONE', ( #14003, #2398, #7681, #13218 ) ) ;
#5553 = CARTESIAN_POINT ( 'NONE',  ( 69.44459735978651338, -3.127033676967585052, 72.52731926747081559 ) ) ;
#5554 = EDGE_CURVE ( 'NONE', #7398, #3301, #6012, .T. ) ;
#5555 = DIRECTION ( 'NONE',  ( -1.000000000000000000, 0.000000000000000000, 0.000000000000000000 ) ) ;
#5556 = ORIENTED_EDGE ( 'NONE', *, *, #2468, .T. ) ;
#5557 = DIRECTION ( 'NONE',  ( 1.000000000000000000, 0.000000000000000000, 0.000000000000000000 ) ) ;
#5558 = ORIENTED_EDGE ( 'NONE', *, *, #12088, .F. ) ;
#5559 = AXIS2_PLACEMENT_3D ( 'NONE', #14865, #9256, #4478 ) ;
#5560 = DIRECTION ( 'NONE',  ( 1.000000000000000000, -0.000000000000000000, -0.000000000000000000 ) ) ;
#5561 = DIRECTION ( 'NONE',  ( -0.000000000000000000, -0.000000000000000000, -1.000000000000000000 ) ) ;
#5562 = ORIENTED_EDGE ( 'NONE', *, *, #14852, .T. ) ;
#5563 = ADVANCED_FACE ( 'NONE', ( #3207 ), #12439, .F. ) ;
#5564 = EDGE_CURVE ( 'NONE', #5126, #12443, #5445, .T. ) ;
#5565 = DIRECTION ( 'NONE',  ( 0.8746197071345573892, -0.4848096202550657430, 0.000000000000000000 ) ) ;
#5566 = CARTESIAN_POINT ( 'NONE',  ( 32.73322375381446392, -55.34783937825962141, 2.956317232382409621 ) ) ;
#5567 = DIRECTION ( 'NONE',  ( 8.673617379884035472E-17, -1.000000000000000000, 0.000000000000000000 ) ) ;
#5568 = VECTOR ( 'NONE', #8603, 1000.000000000000000 ) ;
#5569 = DIRECTION ( 'NONE',  ( -0.000000000000000000, -1.000000000000000000, -1.734723475976817547E-15 ) ) ;
#5570 = TOROIDAL_SURFACE ( 'NONE', #2109, 3.694885682587998765, 0.5000000000000000000 ) ;
#5571 = ORIENTED_EDGE ( 'NONE', *, *, #14502, .F. ) ;
#5572 = ORIENTED_EDGE ( 'NONE', *, *, #1010, .T. ) ;
#5573 = FACE_OUTER_BOUND ( 'NONE', #8073, .T. ) ;
#5574 = ORIENTED_EDGE ( 'NONE', *, *, #12274, .F. ) ;
#5575 = CARTESIAN_POINT ( 'NONE',  ( 25.17147204124252724, -52.24929059928630437, -4.731953141281072028 ) ) ;
#5576 = CARTESIAN_POINT ( 'NONE',  ( 23.84527200824996029, -64.01730164816845559, 6.333338579777401556 ) ) ;
#5577 =( GEOMETRIC_REPRESENTATION_CONTEXT ( 3 ) GLOBAL_UNCERTAINTY_ASSIGNED_CONTEXT ( ( #8290 ) ) GLOBAL_UNIT_ASSIGNED_CONTEXT ( ( #8710, #554, #2948 ) ) REPRESENTATION_CONTEXT ( 'NONE', 'WORKASPACE' ) );
#5578 = ORIENTED_EDGE ( 'NONE', *, *, #2968, .T. ) ;
#5579 = FACE_OUTER_BOUND ( 'NONE', #13006, .T. ) ;
#5580 = CARTESIAN_POINT ( 'NONE',  ( 67.21328690825529861, 25.52935533987996664, -21.00807340887166674 ) ) ;
#5581 = VECTOR ( 'NONE', #10295, 1000.000000000000000 ) ;
#5582 = AXIS2_PLACEMENT_3D ( 'NONE', #3891, #1512, #4979 ) ;
#5583 = CARTESIAN_POINT ( 'NONE',  ( 8.718647472499544193, -59.64543329202603417, -1.841503290196028209 ) ) ;
#5584 = DIRECTION ( 'NONE',  ( -0.000000000000000000, 0.000000000000000000, -1.000000000000000000 ) ) ;
#5585 = CARTESIAN_POINT ( 'NONE',  ( 32.05770958210092658, -60.12777237996190394, 2.859594828286829760 ) ) ;
#5586 = AXIS2_PLACEMENT_3D ( 'NONE', #3603, #223, #9542 ) ;
#5587 = PLANE ( 'NONE',  #10599 ) ;
#5588 = PRODUCT_DEFINITION_FORMATION_WITH_SPECIFIED_SOURCE ( 'ANY', '', #5354, .NOT_KNOWN. ) ;
#5589 = CARTESIAN_POINT ( 'NONE',  ( 18.03113812440135888, -82.24929059928629727, 4.472107801411127959 ) ) ;
#5590 = CIRCLE ( 'NONE', #1415, 4.000000000000003553 ) ;
#5591 = EDGE_CURVE ( 'NONE', #11986, #13749, #13596, .T. ) ;
#5592 = CARTESIAN_POINT ( 'NONE',  ( -12.09280073291247781, -85.24929059928631148, 11.78977872328357357 ) ) ;
#5593 = VERTEX_POINT ( 'NONE', #11673 ) ;
#5594 = CIRCLE ( 'NONE', #14204, 0.7892041907098262810 ) ;
#5595 = CARTESIAN_POINT ( 'NONE',  ( 17.45100281819102150, -72.28366650270582738, -6.113054590618521189 ) ) ;
#5596 = VERTEX_POINT ( 'NONE', #14145 ) ;
#5597 = CARTESIAN_POINT ( 'NONE',  ( -12.99999999999998757, -67.96969602390581144, -115.4621125123531442 ) ) ;
#5598 = ORIENTED_EDGE ( 'NONE', *, *, #12380, .T. ) ;
#5599 = CARTESIAN_POINT ( 'NONE',  ( -25.99999999999998934, -2.249290599286303927, 38.50000000000012790 ) ) ;
#5600 = LINE ( 'NONE', #8137, #11204 ) ;
#5601 = VECTOR ( 'NONE', #6289, 1000.000000000000000 ) ;
#5602 = PLANE ( 'NONE',  #1144 ) ;
#5603 = LINE ( 'NONE', #12678, #2529 ) ;
#5604 = AXIS2_PLACEMENT_3D ( 'NONE', #11264, #1876, #722 ) ;
#5605 = DIRECTION ( 'NONE',  ( 0.9999826067960413400, 0.005897974685767391929, -0.000000000000000000 ) ) ;
#5606 = AXIS2_PLACEMENT_3D ( 'NONE', #10230, #983, #5622 ) ;
#5607 = ORIENTED_EDGE ( 'NONE', *, *, #7153, .T. ) ;
#5608 = DIRECTION ( 'NONE',  ( 1.000000000000000000, -0.000000000000000000, 0.000000000000000000 ) ) ;
#5609 = CARTESIAN_POINT ( 'NONE',  ( 8.094331618521831473, -56.86646964060154374, -2.513983171437783604 ) ) ;
#5610 = CARTESIAN_POINT ( 'NONE',  ( 82.49066175147797253, 12.46743062497963450, 33.00000000000012790 ) ) ;
#5611 = EDGE_CURVE ( 'NONE', #9619, #12270, #7057, .T. ) ;
#5612 = EDGE_CURVE ( 'NONE', #13646, #9532, #5996, .T. ) ;
#5613 = CARTESIAN_POINT ( 'NONE',  ( -9.083879796419006780, -7.373836579503426414, 48.00000000000010658 ) ) ;
#5614 = VERTEX_POINT ( 'NONE', #1054 ) ;
#5615 = CIRCLE ( 'NONE', #2861, 4.194885682587998765 ) ;
#5616 = ORIENTED_EDGE ( 'NONE', *, *, #12795, .F. ) ;
#5617 = CARTESIAN_POINT ( 'NONE',  ( 33.52366768382368889, -57.47994873761392398, 2.501453769636590607 ) ) ;
#5618 = ORIENTED_EDGE ( 'NONE', *, *, #7776, .T. ) ;
#5619 = DIRECTION ( 'NONE',  ( 0.4331347858759544978, 0.9013291614411413910, 0.000000000000000000 ) ) ;
#5620 = AXIS2_PLACEMENT_3D ( 'NONE', #3081, #9003, #5394 ) ;
#5621 = EDGE_LOOP ( 'NONE', ( #9369, #4969, #12453, #6927 ) ) ;
#5622 = DIRECTION ( 'NONE',  ( 0.8746197071345563900, -0.4848096202550675193, 0.000000000000000000 ) ) ;
#5623 = DIRECTION ( 'NONE',  ( 0.000000000000000000, 1.000000000000000000, -0.000000000000000000 ) ) ;
#5624 = DIRECTION ( 'NONE',  ( 0.8746197071345569451, -0.4848096202550666312, 0.000000000000000000 ) ) ;
#5625 = ORIENTED_EDGE ( 'NONE', *, *, #11025, .F. ) ;
#5626 = EDGE_CURVE ( 'NONE', #5719, #14453, #2365, .T. ) ;
#5627 = DIRECTION ( 'NONE',  ( 0.5640065580417802371, -0.8257703085518780517, 0.000000000000000000 ) ) ;
#5628 = FACE_OUTER_BOUND ( 'NONE', #8055, .T. ) ;
#5629 = CARTESIAN_POINT ( 'NONE',  ( 69.46410738159350728, -2.362204130743390085, 75.71883071479155092 ) ) ;
#5630 = AXIS2_PLACEMENT_3D ( 'NONE', #2693, #6248, #7468 ) ;
#5631 = FACE_OUTER_BOUND ( 'NONE', #2303, .T. ) ;
#5632 = CARTESIAN_POINT ( 'NONE',  ( 29.07090146761346716, -50.97757525703124770, 4.214488946663996316 ) ) ;
#5633 = ORIENTED_EDGE ( 'NONE', *, *, #2217, .F. ) ;
#5634 = DIRECTION ( 'NONE',  ( 0.000000000000000000, 0.000000000000000000, 1.000000000000000000 ) ) ;
#5635 = FACE_OUTER_BOUND ( 'NONE', #9920, .T. ) ;
#5636 = ORIENTED_EDGE ( 'NONE', *, *, #4315, .F. ) ;
#5637 = CARTESIAN_POINT ( 'NONE',  ( 23.69232253801245847, -96.56299909827106376, -4.472107801411124406 ) ) ;
#5638 = AXIS2_PLACEMENT_3D ( 'NONE', #12550, #3014, #12396 ) ;
#5639 = LINE ( 'NONE', #14786, #14489 ) ;
#5640 = CARTESIAN_POINT ( 'NONE',  ( -8.842479278987875446, -7.118053859731355182, -48.00000000000012079 ) ) ;
#5641 = DIRECTION ( 'NONE',  ( 0.000000000000000000, 0.000000000000000000, -1.000000000000000000 ) ) ;
#5642 = EDGE_LOOP ( 'NONE', ( #14165, #15, #10939, #8815 ) ) ;
#5643 = LINE ( 'NONE', #8185, #2098 ) ;
#5644 = CARTESIAN_POINT ( 'NONE',  ( 0.000000000000000000, 15.25070940071368497, -33.00000000000012790 ) ) ;
#5645 = CARTESIAN_POINT ( 'NONE',  ( 32.50986371286720100, -54.90226484923775274, 3.064913166935400834 ) ) ;
#5646 = DIRECTION ( 'NONE',  ( 0.005897974685767391929, -0.9999826067960413400, 0.000000000000000000 ) ) ;
#5647 = CIRCLE ( 'NONE', #14718, 1.000000000000000888 ) ;
#5648 =( GEOMETRIC_REPRESENTATION_CONTEXT ( 3 ) GLOBAL_UNCERTAINTY_ASSIGNED_CONTEXT ( ( #13207 ) ) GLOBAL_UNIT_ASSIGNED_CONTEXT ( ( #6778, #1853, #9097 ) ) REPRESENTATION_CONTEXT ( 'NONE', 'WORKASPACE' ) );
#5649 = CARTESIAN_POINT ( 'NONE',  ( 54.86190032082818391, 1.721056973166403603, 48.51982618741349285 ) ) ;
#5650 = EDGE_CURVE ( 'NONE', #14041, #2664, #5979, .T. ) ;
#5651 = ORIENTED_EDGE ( 'NONE', *, *, #4060, .T. ) ;
#5652 = EDGE_LOOP ( 'NONE', ( #2393, #6011, #6291, #6234 ) ) ;
#5653 = PLANE ( 'NONE',  #970 ) ;
#5654 = EDGE_LOOP ( 'NONE', ( #2573, #7902, #4682, #14784, #5364, #8634 ) ) ;
#5655 = EDGE_CURVE ( 'NONE', #7432, #9444, #14680, .T. ) ;
#5656 = DIRECTION ( 'NONE',  ( 1.000000000000000000, 0.000000000000000000, -0.000000000000000000 ) ) ;
#5657 = CARTESIAN_POINT ( 'NONE',  ( 12.08975733950408404, -52.24929059928630437, 3.124130263553816622 ) ) ;
#5658 = EDGE_CURVE ( 'NONE', #5708, #81, #1209, .T. ) ;
#5659 = EDGE_CURVE ( 'NONE', #1111, #4753, #967, .T. ) ;
#5660 = VERTEX_POINT ( 'NONE', #5682 ) ;
#5661 = DIRECTION ( 'NONE',  ( 1.000000000000000000, -0.000000000000000000, 0.000000000000000000 ) ) ;
#5662 = DIRECTION ( 'NONE',  ( -0.000000000000000000, -0.000000000000000000, -1.000000000000000000 ) ) ;
#5663 = AXIS2_PLACEMENT_3D ( 'NONE', #3496, #4801, #14116 ) ;
#5664 = CARTESIAN_POINT ( 'NONE',  ( 8.466388912403534306, -58.63671304798791084, -1.826958385055450274 ) ) ;
#5665 = EDGE_CURVE ( 'NONE', #7521, #3040, #7942, .T. ) ;
#5666 = DIRECTION ( 'NONE',  ( -0.000000000000000000, 1.000000000000000000, 1.445602896647339163E-16 ) ) ;
#5667 = CARTESIAN_POINT ( 'NONE',  ( 33.59228746836564738, -55.86290318049214676, -1.891314907874631190 ) ) ;
#5668 = DIRECTION ( 'NONE',  ( 0.8420378618367728718, 0.5394184268574404584, 0.000000000000000000 ) ) ;
#5669 = LINE ( 'NONE', #9129, #6341 ) ;
#5670 = CARTESIAN_POINT ( 'NONE',  ( -25.34493114703935035, -6.799303420495464323, -48.05421924268924272 ) ) ;
#5671 = VECTOR ( 'NONE', #14857, 1000.000000000000000 ) ;
#5672 = ORIENTED_EDGE ( 'NONE', *, *, #3765, .T. ) ;
#5673 = CARTESIAN_POINT ( 'NONE',  ( 6.812294061964305314, -47.87980016388318205, -2.732839075317959665 ) ) ;
#5674 = ORIENTED_EDGE ( 'NONE', *, *, #4718, .T. ) ;
#5675 = CARTESIAN_POINT ( 'NONE',  ( 32.90197589884652274, -57.33450387999030795, -2.749014434309867916 ) ) ;
#5676 = ORIENTED_EDGE ( 'NONE', *, *, #6454, .F. ) ;
#5677 = DIRECTION ( 'NONE',  ( 1.000000000000000000, 0.000000000000000000, 0.000000000000000000 ) ) ;
#5678 = ADVANCED_FACE ( 'NONE', ( #3594 ), #7258, .T. ) ;
#5679 = CARTESIAN_POINT ( 'NONE',  ( 17.61519226005271577, -69.39711819508866597, -6.201611931792120558 ) ) ;
#5680 = VECTOR ( 'NONE', #13405, 1000.000000000000000 ) ;
#5681 = CARTESIAN_POINT ( 'NONE',  ( 53.41380296247595538, -0.1096349785133995947, 62.84860122826521689 ) ) ;
#5682 = CARTESIAN_POINT ( 'NONE',  ( 67.21328690825529861, 25.52935533987996664, 21.00807340887166674 ) ) ;
#5683 = EDGE_CURVE ( 'NONE', #6506, #5691, #10680, .T. ) ;
#5684 = ORIENTED_EDGE ( 'NONE', *, *, #2459, .T. ) ;
#5685 = CARTESIAN_POINT ( 'NONE',  ( 37.23881781239525424, 23.25070940071368852, 33.00000000000012790 ) ) ;
#5686 = CARTESIAN_POINT ( 'NONE',  ( 9.937529291673584453, -54.06014836395547007, -3.368555242453570298 ) ) ;
#5687 = LINE ( 'NONE', #9226, #14575 ) ;
#5688 = AXIS2_PLACEMENT_3D ( 'NONE', #10989, #5362, #510 ) ;
#5689 = DIRECTION ( 'NONE',  ( 0.3020115420618306734, -0.1674077314120155646, 0.9384901064608606180 ) ) ;
#5690 =( BOUNDED_SURFACE ( )  B_SPLINE_SURFACE ( 3, 2, ( 
 ( #12395, #7346, #7706 ),
 ( #6207, #1420, #13621 ),
 ( #13473, #7779, #4965 ),
 ( #4299, #14620, #12319 ),
 ( #4152, #11163, #11232 ),
 ( #12035, #3802, #8506 ),
 ( #2934, #7626, #5316 ),
 ( #1498, #3012, #10088 ),
 ( #14774, #8930, #10893 ),
 ( #12469, #539, #2316 ),
 ( #3469, #5871, #9086 ),
 ( #7, #1077, #11695 ),
 ( #6930, #11453, #13932 ),
 ( #3232, #10237, #11620 ) ),
 .UNSPECIFIED., .F., .F., .F. ) 
 B_SPLINE_SURFACE_WITH_KNOTS ( ( 4, 2, 2, 2, 2, 2, 4 ),
 ( 3, 3 ),
 ( 0.001417163504557058824, 0.002234205688869395946, 0.002642726781025564291, 0.003051247873181732635, 0.003459768965337900980, 0.003868290057494069758, 0.004685332241806406881 ),
 ( 0.000000000000000000, 1.000000000000000000 ),
 .UNSPECIFIED. ) 
 GEOMETRIC_REPRESENTATION_ITEM ( )  RATIONAL_B_SPLINE_SURFACE ( (
 ( 1.000000000000000000, 0.7071067811865471286, 1.000000000000000000),
 ( 1.000000000000000000, 0.7218508617828192087, 1.000000000000000000),
 ( 1.000000000000000000, 0.7387008909040627680, 1.000000000000000000),
 ( 1.000000000000000000, 0.7647615808954046912, 1.000000000000000000),
 ( 1.000000000000000000, 0.7734065576773767603, 1.000000000000000000),
 ( 1.000000000000000000, 0.7903558204260539011, 1.000000000000000000),
 ( 1.000000000000000000, 0.7987454157985085512, 1.000000000000000000),
 ( 1.000000000000000000, 0.8144265709899989325, 1.000000000000000000),
 ( 1.000000000000000000, 0.8216999247152600994, 1.000000000000000000),
 ( 1.000000000000000000, 0.8348485599607926577, 1.000000000000000000),
 ( 1.000000000000000000, 0.8407795038256219433, 1.000000000000000000),
 ( 1.000000000000000000, 0.8552130772092386701, 1.000000000000000000),
 ( 1.000000000000000000, 0.8606507091652410013, 1.000000000000000000),
 ( 1.000000000000000000, 0.8606282562001379421, 1.000000000000000000) ) ) 
 REPRESENTATION_ITEM ( '' )  SURFACE ( )  );
#5691 = VERTEX_POINT ( 'NONE', #14220 ) ;
#5692 = AXIS2_PLACEMENT_3D ( 'NONE', #2772, #1831, #1613 ) ;
#5693 = DIRECTION ( 'NONE',  ( 0.000000000000000000, 0.000000000000000000, -1.000000000000000000 ) ) ;
#5694 = ORIENTED_EDGE ( 'NONE', *, *, #5504, .F. ) ;
#5695 = CARTESIAN_POINT ( 'NONE',  ( 65.00000000000001421, -85.27429059928630295, 19.99999999999999645 ) ) ;
#5696 = EDGE_CURVE ( 'NONE', #9532, #13060, #3672, .T. ) ;
#5697 = VERTEX_POINT ( 'NONE', #10448 ) ;
#5698 = ORIENTED_EDGE ( 'NONE', *, *, #12136, .T. ) ;
#5699 = VECTOR ( 'NONE', #5047, 1000.000000000000000 ) ;
#5700 = CARTESIAN_POINT ( 'NONE',  ( -7.999999999999986677, -2.249290599286302594, 47.50000000000012079 ) ) ;
#5701 = CARTESIAN_POINT ( 'NONE',  ( -65.00000000000001421, -85.24929059928629727, -22.52499999999999503 ) ) ;
#5702 = EDGE_CURVE ( 'NONE', #14453, #8536, #10393, .T. ) ;
#5703 = CIRCLE ( 'NONE', #3966, 0.4999999999999997780 ) ;
#5704 = EDGE_CURVE ( 'NONE', #9231, #10222, #797, .T. ) ;
#5705 = TOROIDAL_SURFACE ( 'NONE', #14045, 3.999999999999996447, 1.000000000000000000 ) ;
#5706 = LINE ( 'NONE', #3078, #10966 ) ;
#5707 = CARTESIAN_POINT ( 'NONE',  ( -16.99999999999998579, -2.249290599286303927, -50.00000000000012079 ) ) ;
#5708 = VERTEX_POINT ( 'NONE', #9608 ) ;
#5709 = DIRECTION ( 'NONE',  ( 0.000000000000000000, 0.000000000000000000, -1.000000000000000000 ) ) ;
#5710 = DIRECTION ( 'NONE',  ( -1.000000000000000000, -0.000000000000000000, -0.000000000000000000 ) ) ;
#5711 = CARTESIAN_POINT ( 'NONE',  ( 33.47544102892946682, -55.36884115291557862, -1.950692953653574424 ) ) ;
#5712 = DIRECTION ( 'NONE',  ( 0.8746197071345569451, -0.4848096202550666312, 0.000000000000000000 ) ) ;
#5713 = CARTESIAN_POINT ( 'NONE',  ( 23.47466359740176500, -53.10810670090260288, 6.494041865157049287 ) ) ;
#5714 = ORIENTED_EDGE ( 'NONE', *, *, #14074, .T. ) ;
#5715 = CARTESIAN_POINT ( 'NONE',  ( 88.00000000000000000, 23.25070940071369208, 33.00000000000012790 ) ) ;
#5716 = CIRCLE ( 'NONE', #6431, 9.500000000000001776 ) ;
#5717 = CIRCLE ( 'NONE', #9898, 9.000000000000001776 ) ;
#5718 = CARTESIAN_POINT ( 'NONE',  ( -8.563719136935748821, 2.126583234680710977, 48.00000000000012079 ) ) ;
#5719 = VERTEX_POINT ( 'NONE', #4030 ) ;
#5720 = CARTESIAN_POINT ( 'NONE',  ( 58.00000000000000711, -2.249290599286309256, 39.50000000000012790 ) ) ;
#5721 = CARTESIAN_POINT ( 'NONE',  ( 64.11356537587559501, -11.94785244090458498, 75.19766410831374515 ) ) ;
#5722 = ORIENTED_EDGE ( 'NONE', *, *, #11137, .F. ) ;
#5723 = ADVANCED_FACE ( 'NONE', ( #3815 ), #432, .T. ) ;
#5724 = EDGE_CURVE ( 'NONE', #11167, #14965, #7442, .T. ) ;
#5725 = DIRECTION ( 'NONE',  ( 1.000000000000000000, 0.000000000000000000, 0.000000000000000000 ) ) ;
#5726 = CARTESIAN_POINT ( 'NONE',  ( -9.334567670938534789, -7.621465217813490511, -48.02064173568530236 ) ) ;
#5727 = DIRECTION ( 'NONE',  ( 0.000000000000000000, -4.625929269271485914E-16, 1.000000000000000000 ) ) ;
#5728 = EDGE_LOOP ( 'NONE', ( #3902, #10424, #11858, #1298 ) ) ;
#5729 = DIRECTION ( 'NONE',  ( 0.000000000000000000, 1.000000000000000000, -0.000000000000000000 ) ) ;
#5730 = AXIS2_PLACEMENT_3D ( 'NONE', #14763, #3005, #2209 ) ;
#5731 = DIRECTION ( 'NONE',  ( -0.000000000000000000, -0.000000000000000000, 1.000000000000000000 ) ) ;
#5732 = TOROIDAL_SURFACE ( 'NONE', #2239, 4.165819364273509962, 0.5000000000000000000 ) ;
#5733 = CONICAL_SURFACE ( 'NONE', #9405, 2.524999999999999467, 0.7853981633973787790 ) ;
#5734 = DIRECTION ( 'NONE',  ( -0.8420378618367728718, -0.5394184268574404584, 0.000000000000000000 ) ) ;
#5735 = CARTESIAN_POINT ( 'NONE',  ( 31.50836116271761611, -53.84182990103198563, 3.477143273224470033 ) ) ;
#5736 = AXIS2_PLACEMENT_3D ( 'NONE', #9496, #6190, #14263 ) ;
#5737 = CARTESIAN_POINT ( 'NONE',  ( 31.49298359385885959, -60.71197230342421136, -3.050751728647420613 ) ) ;
#5738 = DIRECTION ( 'NONE',  ( 0.8746197071345569451, -0.4848096202550666312, 0.000000000000000000 ) ) ;
#5739 = ORIENTED_EDGE ( 'NONE', *, *, #214, .F. ) ;
#5740 = DIRECTION ( 'NONE',  ( 0.000000000000000000, 0.000000000000000000, -1.000000000000000000 ) ) ;
#5741 = B_SPLINE_CURVE_WITH_KNOTS ( 'NONE', 3,
 ( #13426, #12280, #3120, #8127, #14816, #6734, #9210, #12829 ),
 .UNSPECIFIED., .F., .F.,
 ( 4, 2, 2, 4 ),
 ( 5.291795217412410304E-17, 0.001077686929059509672, 0.002155373858118966434, 0.004310747716237871285 ),
 .UNSPECIFIED. ) ;
#5742 = ORIENTED_EDGE ( 'NONE', *, *, #2357, .F. ) ;
#5743 = LINE ( 'NONE', #5894, #6657 ) ;
#5744 = CARTESIAN_POINT ( 'NONE',  ( -8.787473001628837821, 2.499856724289235554, -48.50000000000012079 ) ) ;
#5745 = AXIS2_PLACEMENT_3D ( 'NONE', #10148, #4440, #1902 ) ;
#5746 = ORIENTED_EDGE ( 'NONE', *, *, #13590, .T. ) ;
#5747 = PLANE ( 'NONE',  #3991 ) ;
#5748 = LINE ( 'NONE', #5580, #11967 ) ;
#5749 = CIRCLE ( 'NONE', #14817, 1.000000000000000888 ) ;
#5750 = LINE ( 'NONE', #9355, #4964 ) ;
#5751 = ADVANCED_FACE ( 'NONE', ( #14291 ), #3962, .F. ) ;
#5752 = CARTESIAN_POINT ( 'NONE',  ( 60.34603303165619792, -7.282908750500069139, 48.51982618741349285 ) ) ;
#5753 = DIRECTION ( 'NONE',  ( 0.000000000000000000, 1.000000000000000000, -0.000000000000000000 ) ) ;
#5754 = DIRECTION ( 'NONE',  ( 1.224646799147353207E-16, 1.000000000000000000, 0.000000000000000000 ) ) ;
#5755 = CIRCLE ( 'NONE', #7213, 0.5000000000000004441 ) ;
#5756 = DIRECTION ( 'NONE',  ( 0.8746197071345569451, -0.4848096202550666312, 0.000000000000000000 ) ) ;
#5757 = DIRECTION ( 'NONE',  ( -0.000000000000000000, -0.000000000000000000, 1.000000000000000000 ) ) ;
#5758 = VECTOR ( 'NONE', #1757, 1000.000000000000000 ) ;
#5759 = VERTEX_POINT ( 'NONE', #13356 ) ;
#5760 = CARTESIAN_POINT ( 'NONE',  ( -16.99999999999998579, 2.256146146571129218, 38.00000000000012079 ) ) ;
#5761 = EDGE_CURVE ( 'NONE', #11670, #7393, #7509, .T. ) ;
#5762 = ORIENTED_EDGE ( 'NONE', *, *, #12795, .T. ) ;
#5763 = ADVANCED_FACE ( 'NONE', ( #2743 ), #2884, .T. ) ;
#5764 = DIRECTION ( 'NONE',  ( 0.000000000000000000, 1.000000000000000000, -0.000000000000000000 ) ) ;
#5765 = ORIENTED_EDGE ( 'NONE', *, *, #10927, .T. ) ;
#5766 = ORIENTED_EDGE ( 'NONE', *, *, #4168, .F. ) ;
#5767 = CARTESIAN_POINT ( 'NONE',  ( 47.27423575335444639, 25.52935533987996664, 33.00000000000012790 ) ) ;
#5768 = CARTESIAN_POINT ( 'NONE',  ( 14.46727374856419246, -52.24929059928630437, -3.946674197044196752 ) ) ;
#5769 = ORIENTED_EDGE ( 'NONE', *, *, #10543, .T. ) ;
#5770 = ADVANCED_FACE ( 'NONE', ( #5055 ), #1589, .F. ) ;
#5771 = EDGE_CURVE ( 'NONE', #12879, #7490, #3995, .T. ) ;
#5772 = CARTESIAN_POINT ( 'NONE',  ( 8.903297316361205915, -55.58238924893039012, -2.909054338253188376 ) ) ;
#5773 = DIRECTION ( 'NONE',  ( 0.000000000000000000, 0.000000000000000000, 1.000000000000000000 ) ) ;
#5774 = CARTESIAN_POINT ( 'NONE',  ( 80.00000000000001421, -72.24929059928631148, 32.99999999999999289 ) ) ;
#5775 = ORIENTED_EDGE ( 'NONE', *, *, #11997, .F. ) ;
#5776 = DIRECTION ( 'NONE',  ( -0.8656763553492622387, -0.5006040828731004311, -0.000000000000000000 ) ) ;
#5777 = ORIENTED_EDGE ( 'NONE', *, *, #9548, .F. ) ;
#5778 = DIRECTION ( 'NONE',  ( -0.000000000000000000, 1.000000000000000000, 1.445602896647339163E-16 ) ) ;
#5779 = EDGE_LOOP ( 'NONE', ( #9554, #5481, #8920, #2894 ) ) ;
#5780 = ORIENTED_EDGE ( 'NONE', *, *, #4897, .T. ) ;
#5781 = CARTESIAN_POINT ( 'NONE',  ( 0.000000000000000000, 21.75070940071319114, 33.00000000000012790 ) ) ;
#5782 = CARTESIAN_POINT ( 'NONE',  ( 0.000000000000000000, 21.75070940071366365, 139.1143251403882459 ) ) ;
#5783 = DIRECTION ( 'NONE',  ( 0.000000000000000000, 0.000000000000000000, -1.000000000000000000 ) ) ;
#5784 = CARTESIAN_POINT ( 'NONE',  ( -8.787473001628837821, 2.499856724289235554, 48.50000000000012079 ) ) ;
#5785 = VERTEX_POINT ( 'NONE', #11046 ) ;
#5786 =( BOUNDED_SURFACE ( )  B_SPLINE_SURFACE ( 3, 2, ( 
 ( #6064, #14377, #9695 ),
 ( #10755, #1517, #4905 ),
 ( #2524, #6223, #7138 ),
 ( #6146, #9610, #13142 ),
 ( #5058, #2444, #7444 ),
 ( #14293, #2594, #8521 ),
 ( #7285, #14448, #10914 ),
 ( #14146, #7366, #1442 ),
 ( #12134, #10829, #3818 ),
 ( #1591, #13219, #9535 ),
 ( #10681, #3595, #8302 ),
 ( #12998, #11825, #289 ),
 ( #1283, #139, #14222 ),
 ( #3673, #8374, #13507 ),
 ( #6428, #9972, #14811 ),
 ( #13423, #11124, #7818 ),
 ( #3116, #8729, #10125 ),
 ( #4184, #14655, #4261 ),
 ( #7587, #1953, #8963 ),
 ( #8664, #7739, #13359 ),
 ( #2817, #12504, #13658 ),
 ( #14585, #581, #1732 ),
 ( #6650, #2888, #12278 ),
 ( #5351, #2972, #5280 ) ),
 .UNSPECIFIED., .F., .F., .F. ) 
 B_SPLINE_SURFACE_WITH_KNOTS ( ( 4, 2, 2, 2, 2, 2, 2, 2, 2, 2, 2, 4 ),
 ( 3, 3 ),
 ( 0.000000000000000000, 0.0007560557787111725275, 0.001512111557422345055, 0.001890139446777931373, 0.002268167336133517474, 0.003024223114844690110, 0.003402251004200276645, 0.003780278893555862746, 0.004158306782911448847, 0.004536334672267034948, 0.005292390450978207150, 0.006048446229689380220 ),
 ( 0.000000000000000000, 1.000000000000000000 ),
 .UNSPECIFIED. ) 
 GEOMETRIC_REPRESENTATION_ITEM ( )  RATIONAL_B_SPLINE_SURFACE ( (
 ( 1.000000000000000000, 0.8250833044923668869, 1.000000000000000000),
 ( 1.000000000000000000, 0.8244629924933065679, 1.000000000000000000),
 ( 1.000000000000000000, 0.8228453557282220387, 1.000000000000000000),
 ( 1.000000000000000000, 0.8179470878185581828, 1.000000000000000000),
 ( 1.000000000000000000, 0.8146336382298446921, 1.000000000000000000),
 ( 1.000000000000000000, 0.8088012687532375455, 1.000000000000000000),
 ( 1.000000000000000000, 0.8067039814524714636, 1.000000000000000000),
 ( 1.000000000000000000, 0.8022097056812382831, 1.000000000000000000),
 ( 1.000000000000000000, 0.7997977307760424370, 1.000000000000000000),
 ( 1.000000000000000000, 0.7922670365022502770, 1.000000000000000000),
 ( 1.000000000000000000, 0.7868330064135669044, 1.000000000000000000),
 ( 1.000000000000000000, 0.7779933494261681570, 1.000000000000000000),
 ( 1.000000000000000000, 0.7749217965224801663, 1.000000000000000000),
 ( 1.000000000000000000, 0.7686646892563575584, 1.000000000000000000),
 ( 1.000000000000000000, 0.7654626812325411311, 1.000000000000000000),
 ( 1.000000000000000000, 0.7588889951603841055, 1.000000000000000000),
 ( 1.000000000000000000, 0.7555173610300115472, 1.000000000000000000),
 ( 1.000000000000000000, 0.7485733441929113274, 1.000000000000000000),
 ( 1.000000000000000000, 0.7449916546359894864, 1.000000000000000000),
 ( 1.000000000000000000, 0.7341394734814182810, 1.000000000000000000),
 ( 1.000000000000000000, 0.7266881283995606511, 1.000000000000000000),
 ( 1.000000000000000000, 0.7111189506802885196, 1.000000000000000000),
 ( 1.000000000000000000, 0.7029851397915053424, 1.000000000000000000),
 ( 1.000000000000000000, 0.6947298545087532418, 1.000000000000000000) ) ) 
 REPRESENTATION_ITEM ( '' )  SURFACE ( )  );
#5787 = CARTESIAN_POINT ( 'NONE',  ( 58.00000000000000711, -2.249290599286311032, 38.50000000000012790 ) ) ;
#5788 = CARTESIAN_POINT ( 'NONE',  ( -24.54316048551696028, -7.158540021523408292, -48.50000000000012079 ) ) ;
#5789 = CARTESIAN_POINT ( 'NONE',  ( 14.11899478931702490, -53.27035316348869998, -4.884032402486384150 ) ) ;
#5790 = CARTESIAN_POINT ( 'NONE',  ( 28.02614528161576857, -65.45139068074421118, 4.123085411919490184 ) ) ;
#5791 = ORIENTED_EDGE ( 'NONE', *, *, #4133, .F. ) ;
#5792 = DIRECTION ( 'NONE',  ( 1.000000000000000000, 8.673617379884027583E-16, 0.000000000000000000 ) ) ;
#5793 = ADVANCED_FACE ( 'NONE', ( #9904 ), #1360, .T. ) ;
#5794 = EDGE_CURVE ( 'NONE', #7261, #13742, #216, .T. ) ;
#5795 = ORIENTED_EDGE ( 'NONE', *, *, #4181, .T. ) ;
#5796 = CARTESIAN_POINT ( 'NONE',  ( 54.21883389619742388, -5.612936290787406968, 48.51982618741349285 ) ) ;
#5797 = DIRECTION ( 'NONE',  ( 0.000000000000000000, 0.000000000000000000, 1.000000000000000000 ) ) ;
#5798 = FACE_OUTER_BOUND ( 'NONE', #12811, .T. ) ;
#5799 = LINE ( 'NONE', #5882, #6447 ) ;
#5800 = B_SPLINE_CURVE_WITH_KNOTS ( 'NONE', 3,
 ( #3508, #9438, #5664, #3424 ),
 .UNSPECIFIED., .F., .F.,
 ( 4, 4 ),
 ( 0.000000000000000000, 0.001771943201165731641 ),
 .UNSPECIFIED. ) ;
#5801 = LINE ( 'NONE', #10417, #9242 ) ;
#5802 = DIRECTION ( 'NONE',  ( 1.000000000000000000, 0.000000000000000000, 0.000000000000000000 ) ) ;
#5803 = CARTESIAN_POINT ( 'NONE',  ( 8.599030766203958009, -59.21224831720011395, 1.832439066039629916 ) ) ;
#5804 = CARTESIAN_POINT ( 'NONE',  ( 28.60819688762819268, -64.14998386712014167, 4.112387283790987169 ) ) ;
#5805 = CARTESIAN_POINT ( 'NONE',  ( -9.271822474830662131, -6.861803161813125662, -47.50000000000012079 ) ) ;
#5806 = DIRECTION ( 'NONE',  ( -0.2475627213817241101, 0.9688718692283695422, 0.000000000000000000 ) ) ;
#5807 = EDGE_CURVE ( 'NONE', #12792, #505, #2593, .T. ) ;
#5808 = ADVANCED_FACE ( 'NONE', ( #8588 ), #11973, .F. ) ;
#5809 = VERTEX_POINT ( 'NONE', #4980 ) ;
#5810 = AXIS2_PLACEMENT_3D ( 'NONE', #12391, #1769, #10009 ) ;
#5811 = DIRECTION ( 'NONE',  ( 1.000000000000000000, 0.000000000000000000, 0.000000000000000000 ) ) ;
#5812 = EDGE_LOOP ( 'NONE', ( #3888, #11324, #5739, #8717, #10690 ) ) ;
#5813 = CARTESIAN_POINT ( 'NONE',  ( 64.90552635791956959, 22.43695620243006772, 33.00000000000012790 ) ) ;
#5814 = PLANE ( 'NONE',  #10374 ) ;
#5815 = ORIENTED_EDGE ( 'NONE', *, *, #8146, .T. ) ;
#5816 = CARTESIAN_POINT ( 'NONE',  ( 65.00000000000001421, -85.27429059928630295, 17.49999999999999645 ) ) ;
#5817 = CARTESIAN_POINT ( 'NONE',  ( 62.14930354033766946, 1.441842398587373619, 54.56811043785582882 ) ) ;
#5818 = LINE ( 'NONE', #6805, #4455 ) ;
#5819 = CIRCLE ( 'NONE', #14419, 4.194885682587998765 ) ;
#5820 = PLANE ( 'NONE',  #6330 ) ;
#5821 = LINE ( 'NONE', #15203, #13975 ) ;
#5822 = LINE ( 'NONE', #10513, #513 ) ;
#5823 = ADVANCED_FACE ( 'NONE', ( #9690 ), #14375, .T. ) ;
#5824 = DIRECTION ( 'NONE',  ( 0.000000000000000000, 0.000000000000000000, 1.000000000000000000 ) ) ;
#5825 = CARTESIAN_POINT ( 'NONE',  ( 23.69232253801246557, -85.24929059928631148, -4.472107801411126182 ) ) ;
#5826 = ORIENTED_EDGE ( 'NONE', *, *, #2460, .F. ) ;
#5827 = CARTESIAN_POINT ( 'NONE',  ( 112.9262740340969060, 23.25070940071369563, 13.14990448602692474 ) ) ;
#5828 = UNCERTAINTY_MEASURE_WITH_UNIT (LENGTH_MEASURE( 1.000000000000000082E-05 ), #8761, 'distance_accuracy_value', 'NONE');
#5829 = ORIENTED_EDGE ( 'NONE', *, *, #11146, .F. ) ;
#5830 = LINE ( 'NONE', #8368, #14764 ) ;
#5831 = VECTOR ( 'NONE', #3907, 1000.000000000000000 ) ;
#5832 = VERTEX_POINT ( 'NONE', #6221 ) ;
#5833 = CARTESIAN_POINT ( 'NONE',  ( 13.63626254758702849, -65.28118056119571122, -4.304032224033864651 ) ) ;
#5834 = ORIENTED_EDGE ( 'NONE', *, *, #284, .F. ) ;
#5835 = DIRECTION ( 'NONE',  ( -0.8208219420614785156, 0.4549890321264269399, 0.3453061251629920836 ) ) ;
#5836 = DIRECTION ( 'NONE',  ( -0.000000000000000000, 1.000000000000000000, 1.445602896647339163E-16 ) ) ;
#5837 = B_SPLINE_CURVE_WITH_KNOTS ( 'NONE', 3,
 ( #884, #8056, #13592, #6895 ),
 .UNSPECIFIED., .F., .F.,
 ( 4, 4 ),
 ( 0.000000000000000000, 0.0009656645577509051157 ),
 .UNSPECIFIED. ) ;
#5838 = DIRECTION ( 'NONE',  ( -0.000000000000000000, 1.000000000000000000, -0.000000000000000000 ) ) ;
#5839 = ORIENTED_EDGE ( 'NONE', *, *, #5245, .T. ) ;
#5840 = AXIS2_PLACEMENT_3D ( 'NONE', #370, #299, #8465 ) ;
#5841 = ORIENTED_EDGE ( 'NONE', *, *, #1611, .T. ) ;
#5842 = AXIS2_PLACEMENT_3D ( 'NONE', #6307, #14469, #5149 ) ;
#5843 = TOROIDAL_SURFACE ( 'NONE', #14441, 8.500000000000000000, 0.5000000000000000000 ) ;
#5844 = FACE_OUTER_BOUND ( 'NONE', #9007, .T. ) ;
#5845 = LINE ( 'NONE', #1127, #3882 ) ;
#5846 = CARTESIAN_POINT ( 'NONE',  ( -2.688903428702175252E-15, 23.25070940071368142, 139.1143251403882459 ) ) ;
#5847 = CARTESIAN_POINT ( 'NONE',  ( -9.619661834299611414, -7.413097564672328055, 47.90685900409895481 ) ) ;
#5848 = ORIENTED_EDGE ( 'NONE', *, *, #5916, .F. ) ;
#5849 = ORIENTED_EDGE ( 'NONE', *, *, #13360, .F. ) ;
#5850 = CARTESIAN_POINT ( 'NONE',  ( 24.62796245282055452, -82.24929059928629727, 1.347403282660977419 ) ) ;
#5851 = ORIENTED_EDGE ( 'NONE', *, *, #13281, .T. ) ;
#5852 = DIRECTION ( 'NONE',  ( 0.000000000000000000, 0.000000000000000000, 1.000000000000000000 ) ) ;
#5853 = VECTOR ( 'NONE', #9051, 1000.000000000000000 ) ;
#5854 = PRODUCT_DEFINITION_FORMATION_WITH_SPECIFIED_SOURCE ( 'ANY', '', #6577, .NOT_KNOWN. ) ;
#5855 = ORIENTED_EDGE ( 'NONE', *, *, #6742, .T. ) ;
#5856 = TOROIDAL_SURFACE ( 'NONE', #10756, 6.000000000000000000, 1.000000000000000000 ) ;
#5857 = ORIENTED_EDGE ( 'NONE', *, *, #6589, .F. ) ;
#5858 = EDGE_CURVE ( 'NONE', #14041, #5809, #2543, .T. ) ;
#5859 = EDGE_CURVE ( 'NONE', #11327, #8779, #4987, .T. ) ;
#5860 = CIRCLE ( 'NONE', #10519, 0.7892041907098275022 ) ;
#5861 = EDGE_CURVE ( 'NONE', #10116, #11668, #5029, .T. ) ;
#5862 = LINE ( 'NONE', #14159, #3845 ) ;
#5863 = LINE ( 'NONE', #1224, #4485 ) ;
#5864 = VERTEX_POINT ( 'NONE', #13259 ) ;
#5865 = LINE ( 'NONE', #5934, #7423 ) ;
#5866 = CARTESIAN_POINT ( 'NONE',  ( 70.01073691755573236, -3.266485040426043263, 72.83188032674053147 ) ) ;
#5867 = VERTEX_POINT ( 'NONE', #14416 ) ;
#5868 = EDGE_CURVE ( 'NONE', #8531, #3355, #3518, .T. ) ;
#5869 = VECTOR ( 'NONE', #11366, 1000.000000000000000 ) ;
#5870 = DIRECTION ( 'NONE',  ( 0.000000000000000000, 1.000000000000000000, 0.000000000000000000 ) ) ;
#5871 = CARTESIAN_POINT ( 'NONE',  ( 64.77045472790173619, -11.51823327494775384, 72.60588509441274141 ) ) ;
#5872 = CARTESIAN_POINT ( 'NONE',  ( 25.17147204124927029, -52.24929059928630437, 4.731953141288176568 ) ) ;
#5873 = CARTESIAN_POINT ( 'NONE',  ( 27.87264666873679175, -68.05329818758237082, 4.069437918050730296 ) ) ;
#5874 = CIRCLE ( 'NONE', #3642, 0.9999999999999957812 ) ;
#5875 = ORIENTED_EDGE ( 'NONE', *, *, #3201, .F. ) ;
#5876 = CARTESIAN_POINT ( 'NONE',  ( 69.36577990805442084, -3.791597611828531278, 72.16308916778781679 ) ) ;
#5877 = ORIENTED_EDGE ( 'NONE', *, *, #5868, .F. ) ;
#5878 = DIRECTION ( 'NONE',  ( 0.000000000000000000, 0.000000000000000000, 1.000000000000000000 ) ) ;
#5879 = DIRECTION ( 'NONE',  ( 1.000000000000000000, 0.000000000000000000, 0.000000000000000000 ) ) ;
#5880 = B_SPLINE_CURVE_WITH_KNOTS ( 'NONE', 3,
 ( #8628, #11302, #5315, #14699, #4151, #7704 ),
 .UNSPECIFIED., .F., .F.,
 ( 4, 2, 4 ),
 ( 0.000000000000000000, 0.0003908577252344195446, 0.0007817154504688390891 ),
 .UNSPECIFIED. ) ;
#5881 = LINE ( 'NONE', #2326, #1176 ) ;
#5882 = CARTESIAN_POINT ( 'NONE',  ( -20.99999999999998579, -2.249290599286303483, -47.31370849898487307 ) ) ;
#5883 = ORIENTED_EDGE ( 'NONE', *, *, #13987, .T. ) ;
#5884 = DIRECTION ( 'NONE',  ( -0.8420378618367728718, -0.5394184268574404584, -0.000000000000000000 ) ) ;
#5885 = LINE ( 'NONE', #10644, #6052 ) ;
#5886 = EDGE_CURVE ( 'NONE', #11505, #12456, #2485, .T. ) ;
#5887 = CARTESIAN_POINT ( 'NONE',  ( 18.00000000000001066, 15.25070940071368497, 139.1143251403882459 ) ) ;
#5888 = CARTESIAN_POINT ( 'NONE',  ( 119.4687373431154782, -36.32196809074999777, 57.22220354671986087 ) ) ;
#5889 = CYLINDRICAL_SURFACE ( 'NONE', #964, 0.5000000000000000000 ) ;
#5890 = DIRECTION ( 'NONE',  ( 0.000000000000000000, 0.000000000000000000, 1.000000000000000000 ) ) ;
#5891 = ORIENTED_EDGE ( 'NONE', *, *, #6605, .F. ) ;
#5892 = DIRECTION ( 'NONE',  ( 0.000000000000000000, 0.000000000000000000, 1.000000000000000000 ) ) ;
#5893 = ORIENTED_EDGE ( 'NONE', *, *, #15185, .T. ) ;
#5894 = CARTESIAN_POINT ( 'NONE',  ( -2.016677571526633510E-15, 23.25070940071368497, -33.00000000000012790 ) ) ;
#5895 = DIRECTION ( 'NONE',  ( 0.000000000000000000, 1.000000000000000000, 0.000000000000000000 ) ) ;
#5896 = LINE ( 'NONE', #40, #7060 ) ;
#5897 = DIRECTION ( 'NONE',  ( -1.000000000000000000, 0.000000000000000000, 0.000000000000000000 ) ) ;
#5898 = EDGE_CURVE ( 'NONE', #15116, #9700, #10720, .T. ) ;
#5899 = EDGE_CURVE ( 'NONE', #4896, #9073, #8191, .T. ) ;
#5900 = AXIS2_PLACEMENT_3D ( 'NONE', #6538, #7780, #4389 ) ;
#5901 = CIRCLE ( 'NONE', #6613, 1.000000000000000666 ) ;
#5902 = CARTESIAN_POINT ( 'NONE',  ( 33.00481318991428736, -59.64543329202602706, 1.841503290196059517 ) ) ;
#5903 = DIRECTION ( 'NONE',  ( -0.000000000000000000, -0.000000000000000000, -1.000000000000000000 ) ) ;
#5904 = CARTESIAN_POINT ( 'NONE',  ( 69.97972559857382180, -3.172990593254279457, 73.19766410831374515 ) ) ;
#5905 = B_SPLINE_CURVE_WITH_KNOTS ( 'NONE', 3,
 ( #3859, #2712, #7331, #4947, #10953, #11942, #399, #4875, #5100, #2791, #3712, #4797, #9806, #6113, #14347, #14189, #180, #7484, #3792, #12172, #8497, #13036, #9580 ),
 .UNSPECIFIED., .F., .F.,
 ( 4, 2, 2, 2, 2, 1, 2, 2, 2, 2, 2, 4 ),
 ( 3.576224061345498009E-18, 0.0009749202549226092772, 0.001949840509845214868, 0.002924760764767838674, 0.003412220892229137024, 0.003899681019690434940, 0.004387141147151732423, 0.004874601274613029472, 0.005849521529535599285, 0.006336981656996893732, 0.006824441784458187311, 0.007799362039380776206 ),
 .UNSPECIFIED. ) ;
#5906 = LINE ( 'NONE', #11809, #1800 ) ;
#5907 = CARTESIAN_POINT ( 'NONE',  ( 29.69047892279255763, -53.28399145779481216, 4.141535524925023637 ) ) ;
#5908 = ORIENTED_EDGE ( 'NONE', *, *, #8333, .F. ) ;
#5909 = DIRECTION ( 'NONE',  ( -0.8746197071345569451, 0.4848096202550666312, 0.000000000000000000 ) ) ;
#5910 = ORIENTED_EDGE ( 'NONE', *, *, #9078, .T. ) ;
#5911 = FACE_OUTER_BOUND ( 'NONE', #14981, .T. ) ;
#5912 = ORIENTED_EDGE ( 'NONE', *, *, #3952, .T. ) ;
#5913 = ORIENTED_EDGE ( 'NONE', *, *, #3677, .T. ) ;
#5914 = CARTESIAN_POINT ( 'NONE',  ( 64.11356537587560922, -11.94785244090458853, 75.19766410831373094 ) ) ;
#5915 = CARTESIAN_POINT ( 'NONE',  ( 58.00000000000000711, -2.249290599286309256, 81.40005259842790508 ) ) ;
#5916 = EDGE_CURVE ( 'NONE', #12879, #5460, #3750, .T. ) ;
#5917 = EDGE_CURVE ( 'NONE', #5016, #4237, #8346, .T. ) ;
#5918 = DIRECTION ( 'NONE',  ( -0.000000000000000000, -0.000000000000000000, -1.000000000000000000 ) ) ;
#5919 = ORIENTED_EDGE ( 'NONE', *, *, #13830, .F. ) ;
#5920 = VECTOR ( 'NONE', #5440, 1000.000000000000000 ) ;
#5921 = CARTESIAN_POINT ( 'NONE',  ( 8.599030766203956233, -59.21224831720010684, -1.832439066040420617 ) ) ;
#5922 = DIRECTION ( 'NONE',  ( -1.239088197126290570E-16, 1.000000000000000000, 0.000000000000000000 ) ) ;
#5923 = DIRECTION ( 'NONE',  ( 1.000000000000000000, 0.000000000000000000, 0.000000000000000000 ) ) ;
#5924 = VERTEX_POINT ( 'NONE', #3645 ) ;
#5925 = ORIENTED_EDGE ( 'NONE', *, *, #10744, .F. ) ;
#5926 = DIRECTION ( 'NONE',  ( 1.000000000000000000, 0.000000000000000000, 0.000000000000000000 ) ) ;
#5927 = VERTEX_POINT ( 'NONE', #6035 ) ;
#5928 = DIRECTION ( 'NONE',  ( 0.000000000000000000, 0.000000000000000000, 1.000000000000000000 ) ) ;
#5929 = VERTEX_POINT ( 'NONE', #6263 ) ;
#5930 = ORIENTED_EDGE ( 'NONE', *, *, #14122, .T. ) ;
#5931 = CARTESIAN_POINT ( 'NONE',  ( -23.68126483017411488, 3.790603994468874749, -47.74939190649463683 ) ) ;
#5932 = CARTESIAN_POINT ( 'NONE',  ( 53.19261734817368392, 0.4154851184807626940, 87.40005259842790508 ) ) ;
#5933 = ORIENTED_EDGE ( 'NONE', *, *, #7402, .F. ) ;
#5934 = CARTESIAN_POINT ( 'NONE',  ( -80.00000000000001421, -87.24929059928631148, -35.00000000000000000 ) ) ;
#5935 = PRODUCT ( 'Bench-Mounted Base Unit', 'Bench-Mounted Base Unit', '', ( #9939 ) ) ;
#5936 = DIRECTION ( 'NONE',  ( 0.9628490124547428586, -0.2700403288676087032, 0.000000000000000000 ) ) ;
#5937 = EDGE_CURVE ( 'NONE', #2517, #4392, #5905, .T. ) ;
#5938 = ORIENTED_EDGE ( 'NONE', *, *, #13409, .T. ) ;
#5939 = AXIS2_PLACEMENT_3D ( 'NONE', #9440, #10815, #4966 ) ;
#5940 = CARTESIAN_POINT ( 'NONE',  ( 67.15257324181105503, -7.322644791425995336, 82.40005259842790508 ) ) ;
#5941 = CARTESIAN_POINT ( 'NONE',  ( -80.00000000000001421, -72.24929059928631148, -32.99999999999999289 ) ) ;
#5942 = EDGE_CURVE ( 'NONE', #13455, #12270, #14570, .T. ) ;
#5943 = DIRECTION ( 'NONE',  ( 0.000000000000000000, 1.000000000000000000, -0.000000000000000000 ) ) ;
#5944 = ORIENTED_EDGE ( 'NONE', *, *, #4515, .F. ) ;
#5945 = EDGE_CURVE ( 'NONE', #14442, #2373, #12674, .T. ) ;
#5946 = CARTESIAN_POINT ( 'NONE',  ( 70.17101333207268965, -3.861229032418910467, 72.32404137764891061 ) ) ;
#5947 = CIRCLE ( 'NONE', #11827, 4.496540510819673209 ) ;
#5948 = VERTEX_POINT ( 'NONE', #7861 ) ;
#5949 = PLANE ( 'NONE',  #9146 ) ;
#5950 = LINE ( 'NONE', #9569, #3098 ) ;
#5951 = EDGE_CURVE ( 'NONE', #10536, #2336, #13228, .T. ) ;
#5952 = ORIENTED_EDGE ( 'NONE', *, *, #4655, .F. ) ;
#5953 = VECTOR ( 'NONE', #5279, 1000.000000000000000 ) ;
#5954 = AXIS2_PLACEMENT_3D ( 'NONE', #6032, #26, #14185 ) ;
#5955 = CARTESIAN_POINT ( 'NONE',  ( -33.07225206673494711, -1.856991049495498425, 48.00000000000012079 ) ) ;
#5956 = ORIENTED_EDGE ( 'NONE', *, *, #3727, .T. ) ;
#5957 = CARTESIAN_POINT ( 'NONE',  ( -8.679783256197868724, 2.339454207888506776, -48.10016682092218332 ) ) ;
#5958 = CARTESIAN_POINT ( 'NONE',  ( 32.84819715060689305, -60.06858080083488005, -1.862453320359561237 ) ) ;
#5960 = LINE ( 'NONE', #12957, #9802 ) ;
#5959 = APPLICATION_CONTEXT ( 'automotive_design' ) ;
#5961 = CARTESIAN_POINT ( 'NONE',  ( 30.84984438469776080, -61.21666426766278590, 3.284656216408393448 ) ) ;
#5962 = CIRCLE ( 'NONE', #10120, 31.00000000000000000 ) ;
#5963 = EDGE_CURVE ( 'NONE', #11368, #307, #12551, .T. ) ;
#5964 = CARTESIAN_POINT ( 'NONE',  ( -16.99999999999998579, -2.249290599286303927, 58.00000000000012079 ) ) ;
#5965 = CARTESIAN_POINT ( 'NONE',  ( 30.63367540318802185, -53.42148821037872608, -3.802824752090919525 ) ) ;
#5966 = EDGE_CURVE ( 'NONE', #6435, #14286, #4301, .T. ) ;
#5967 = ORIENTED_EDGE ( 'NONE', *, *, #12555, .T. ) ;
#5968 = CARTESIAN_POINT ( 'NONE',  ( 114.6731053250840233, 0.000000000000000000, 139.1143251403882459 ) ) ;
#5969 = ORIENTED_EDGE ( 'NONE', *, *, #13140, .F. ) ;
#5970 = CARTESIAN_POINT ( 'NONE',  ( 10.24895915366353272, -52.80093712146414475, -2.610064308312609604 ) ) ;
#5971 = CARTESIAN_POINT ( 'NONE',  ( -12.99999999999998757, -2.249290599286301706, -32.99999999999987921 ) ) ;
#5972 = MECHANICAL_DESIGN_GEOMETRIC_PRESENTATION_REPRESENTATION (  '', ( #11112 ), #8430 ) ;
#5973 = LINE ( 'NONE', #3721, #1297 ) ;
#5974 = CARTESIAN_POINT ( 'NONE',  ( 87.44800360084714441, -24.28935588223203723, -34.74844256990415658 ) ) ;
#5975 = AXIS2_PLACEMENT_3D ( 'NONE', #14120, #39, #8502 ) ;
#5976 = VECTOR ( 'NONE', #8491, 1000.000000000000000 ) ;
#5977 = LINE ( 'NONE', #1262, #11461 ) ;
#5978 = SURFACE_STYLE_FILL_AREA ( #1264 ) ;
#5979 = CIRCLE ( 'NONE', #14560, 5.165819364273509073 ) ;
#5980 = DIRECTION ( 'NONE',  ( 0.000000000000000000, 0.000000000000000000, 1.000000000000000000 ) ) ;
#5981 = CARTESIAN_POINT ( 'NONE',  ( -25.01741698508091005, -6.338425579613558014, 47.50000000000012079 ) ) ;
#5982 = FACE_OUTER_BOUND ( 'NONE', #13349, .T. ) ;
#5983 = CIRCLE ( 'NONE', #11867, 0.7892041907098262810 ) ;
#5984 = CARTESIAN_POINT ( 'NONE',  ( 32.91088840096362844, -55.94973218888504363, 2.850075077558247738 ) ) ;
#5985 = ORIENTED_EDGE ( 'NONE', *, *, #8091, .T. ) ;
#5986 = CARTESIAN_POINT ( 'NONE',  ( -26.99999999999998224, -72.24929059928616937, 33.00000000000000000 ) ) ;
#5987 = PRODUCT_DEFINITION_CONTEXT ( 'detailed design', #8511, 'design' ) ;
#5988 = EDGE_CURVE ( 'NONE', #7142, #13514, #13836, .T. ) ;
#5989 = AXIS2_PLACEMENT_3D ( 'NONE', #9759, #14445, #3892 ) ;
#5990 = VERTEX_POINT ( 'NONE', #6476 ) ;
#5991 = LINE ( 'NONE', #13982, #7682 ) ;
#5992 = EDGE_LOOP ( 'NONE', ( #6152, #11893, #2662, #5829 ) ) ;
#5993 = ORIENTED_EDGE ( 'NONE', *, *, #14627, .T. ) ;
#5994 = CARTESIAN_POINT ( 'NONE',  ( 64.61411691182246386, -11.63232581036083246, 75.19766410831375936 ) ) ;
#5995 = CARTESIAN_POINT ( 'NONE',  ( 32.39917484285220439, 21.75070940071312364, -33.00000000000012790 ) ) ;
#5996 = LINE ( 'NONE', #8373, #3986 ) ;
#5997 = ORIENTED_EDGE ( 'NONE', *, *, #9565, .F. ) ;
#5998 = AXIS2_PLACEMENT_3D ( 'NONE', #383, #9783, #3696 ) ;
#5999 = CARTESIAN_POINT ( 'NONE',  ( -32.80254285330629216, -2.278009980413787439, 57.50000000000012079 ) ) ;
#6000 = CARTESIAN_POINT ( 'NONE',  ( 32.52281604437752804, -59.06479067038042530, -2.757123406422443690 ) ) ;
#6001 = VERTEX_POINT ( 'NONE', #6395 ) ;
#6002 = ORIENTED_EDGE ( 'NONE', *, *, #2019, .T. ) ;
#6003 = EDGE_CURVE ( 'NONE', #5415, #11647, #14703, .T. ) ;
#6004 = B_SPLINE_CURVE_WITH_KNOTS ( 'NONE', 3,
 ( #2341, #9503, #7185, #14040, #10428, #11648, #5970, #3498, #6877, #10657, #11724, #6041, #9269, #3419, #2421, #8036, #3570, #10501, #8115, #14197 ),
 .UNSPECIFIED., .F., .F.,
 ( 4, 2, 2, 2, 2, 2, 2, 2, 2, 4 ),
 ( 0.000000000000000000, 0.0008540696272735388275, 0.001708139254547077655, 0.002562208881820616374, 0.003416278509094155310, 0.004270348136367694246, 0.005124417763641232748, 0.005978487390914772118, 0.006405522204551540935, 0.006832557018188310620 ),
 .UNSPECIFIED. ) ;
#6005 = LINE ( 'NONE', #3823, #904 ) ;
#6006 = PRODUCT_RELATED_PRODUCT_CATEGORY ( 'part', '', ( #7821 ) ) ;
#6007 = VERTEX_POINT ( 'NONE', #1996 ) ;
#6008 = DIRECTION ( 'NONE',  ( 0.2245701561649796896, 0.9744137433416110161, -0.009279102705851381694 ) ) ;
#6009 = EDGE_LOOP ( 'NONE', ( #14756, #14959, #6945, #498, #511, #9502, #6783, #1450, #1469, #12895 ) ) ;
#6010 = CARTESIAN_POINT ( 'NONE',  ( 28.07070997989108108, -65.32322779890030517, 4.310009693574651024 ) ) ;
#6011 = ORIENTED_EDGE ( 'NONE', *, *, #1928, .F. ) ;
#6012 = CIRCLE ( 'NONE', #7965, 1.000000000000000888 ) ;
#6013 = LINE ( 'NONE', #12934, #2624 ) ;
#6014 = PLANE ( 'NONE',  #14586 ) ;
#6015 = EDGE_LOOP ( 'NONE', ( #8608, #6018, #11330, #817 ) ) ;
#6016 = LINE ( 'NONE', #7154, #6670 ) ;
#6017 = DIRECTION ( 'NONE',  ( 0.000000000000000000, 0.7071067811865965336, 0.7071067811864985009 ) ) ;
#6018 = ORIENTED_EDGE ( 'NONE', *, *, #7070, .T. ) ;
#6019 = CARTESIAN_POINT ( 'NONE',  ( 62.00000000000001421, -2.249290599286310588, 36.00000000000012079 ) ) ;
#6020 = CARTESIAN_POINT ( 'NONE',  ( 23.10474973039556801, -52.24929059928630437, -5.564967562786268473 ) ) ;
#6021 = DIRECTION ( 'NONE',  ( 1.000000000000000000, 0.000000000000000000, 0.000000000000000000 ) ) ;
#6022 = EDGE_LOOP ( 'NONE', ( #11568, #4224, #5607, #12440 ) ) ;
#6023 = CARTESIAN_POINT ( 'NONE',  ( -24.91612020358099855, 2.875255380930533455, 48.00000000000010658 ) ) ;
#6024 = VERTEX_POINT ( 'NONE', #3083 ) ;
#6025 = DIRECTION ( 'NONE',  ( -0.000000000000000000, 0.000000000000000000, -1.000000000000000000 ) ) ;
#6026 = CARTESIAN_POINT ( 'NONE',  ( -3.190546569013415379, 0.8906624217387615339, -57.50000000000012079 ) ) ;
#6027 = ORIENTED_EDGE ( 'NONE', *, *, #8670, .T. ) ;
#6028 = DIRECTION ( 'NONE',  ( 0.000000000000000000, 0.000000000000000000, 1.000000000000000000 ) ) ;
#6029 = DIRECTION ( 'NONE',  ( 1.000000000000000000, -1.214306433183763862E-14, 0.000000000000000000 ) ) ;
#6030 = ORIENTED_EDGE ( 'NONE', *, *, #11161, .T. ) ;
#6031 = CARTESIAN_POINT ( 'NONE',  ( -9.263396839842437558, 2.349907881949450772, -47.70033363922482295 ) ) ;
#6032 = CARTESIAN_POINT ( 'NONE',  ( 76.14589960879429498, -7.734310727912404815, 75.19766410831374515 ) ) ;
#6033 = PLANE ( 'NONE',  #12984 ) ;
#6034 = CARTESIAN_POINT ( 'NONE',  ( 27.32685322894730717, -68.54652648479488164, 4.542640093672140722 ) ) ;
#6035 = CARTESIAN_POINT ( 'NONE',  ( 100.1541764164548880, 23.25070940071369208, 33.00000000000012790 ) ) ;
#6036 = EDGE_CURVE ( 'NONE', #4463, #3566, #5151, .T. ) ;
#6037 = CARTESIAN_POINT ( 'NONE',  ( 30.30862891391975467, -52.33251913750448381, -3.960984348906268160 ) ) ;
#6038 = ORIENTED_EDGE ( 'NONE', *, *, #7880, .T. ) ;
#6039 = DIRECTION ( 'NONE',  ( 0.8746197071345563900, -0.4848096202550675193, 0.000000000000000000 ) ) ;
#6040 = ORIENTED_EDGE ( 'NONE', *, *, #14629, .T. ) ;
#6041 = CARTESIAN_POINT ( 'NONE',  ( 8.674208537763544058, -54.35285673107798488, -2.119592934168749387 ) ) ;
#6042 = DIRECTION ( 'NONE',  ( 0.000000000000000000, 0.000000000000000000, 1.000000000000000000 ) ) ;
#6043 = PLANE ( 'NONE',  #13108 ) ;
#6044 = DIRECTION ( 'NONE',  ( -1.000000000000000000, -8.673617379884035472E-17, 0.000000000000000000 ) ) ;
#6045 = EDGE_CURVE ( 'NONE', #2221, #5382, #9948, .T. ) ;
#6046 = EDGE_CURVE ( 'NONE', #10383, #13135, #8439, .T. ) ;
#6047 = DIRECTION ( 'NONE',  ( -0.000000000000000000, 1.000000000000000000, 1.445602896647339163E-16 ) ) ;
#6048 = CARTESIAN_POINT ( 'NONE',  ( 62.67308791069655882, 25.52935533987996664, 33.00000000000014211 ) ) ;
#6049 = CARTESIAN_POINT ( 'NONE',  ( 65.71319926014255941, -10.73129157630437547, 71.19766410831374515 ) ) ;
#6050 = CARTESIAN_POINT ( 'NONE',  ( -25.24934951899391322, -6.946659123520668722, 48.24789848114230040 ) ) ;
#6051 = CIRCLE ( 'NONE', #1854, 8.500000000000000000 ) ;
#6052 = VECTOR ( 'NONE', #3484, 1000.000000000000000 ) ;
#6053 = CARTESIAN_POINT ( 'NONE',  ( 30.88740069622253515, -52.52081589074940382, 2.777424068827982317 ) ) ;
#6054 = ORIENTED_EDGE ( 'NONE', *, *, #8949, .F. ) ;
#6055 = CARTESIAN_POINT ( 'NONE',  ( 108.0866310645538562, 0.000000000000000000, 33.00000000000012790 ) ) ;
#6056 = ORIENTED_EDGE ( 'NONE', *, *, #13504, .T. ) ;
#6057 = LINE ( 'NONE', #14216, #1263 ) ;
#6058 = VERTEX_POINT ( 'NONE', #5169 ) ;
#6059 = CARTESIAN_POINT ( 'NONE',  ( 66.10056138690445948, -11.60665394596473021, 76.17249640597626126 ) ) ;
#6060 = DIRECTION ( 'NONE',  ( -0.000000000000000000, -0.000000000000000000, -1.000000000000000000 ) ) ;
#6061 = CIRCLE ( 'NONE', #6780, 0.7892041907098262810 ) ;
#6062 = DIRECTION ( 'NONE',  ( -0.000000000000000000, -0.000000000000000000, -1.000000000000000000 ) ) ;
#6063 = ORIENTED_EDGE ( 'NONE', *, *, #6904, .T. ) ;
#6064 = CARTESIAN_POINT ( 'NONE',  ( 8.821484763567296383, -57.33450387999030795, 2.749014434309866584 ) ) ;
#6065 = EDGE_CURVE ( 'NONE', #7654, #6506, #5483, .T. ) ;
#6066 = CARTESIAN_POINT ( 'NONE',  ( 30.65234355186507997, 0.000000000000000000, 33.00000000000012790 ) ) ;
#6067 = CARTESIAN_POINT ( 'NONE',  ( 59.12196317473677709, -7.688259372168277928, 54.56811043785583593 ) ) ;
#6068 = VECTOR ( 'NONE', #12073, 1000.000000000000000 ) ;
#6069 = EDGE_LOOP ( 'NONE', ( #3184, #3890, #14672, #2203 ) ) ;
#6070 = ORIENTED_EDGE ( 'NONE', *, *, #1124, .F. ) ;
#6071 = B_SPLINE_CURVE_WITH_KNOTS ( 'NONE', 3,
 ( #6786, #11477, #1935, #3330, #8026, #6556, #4319, #12728, #2177, #701 ),
 .UNSPECIFIED., .F., .F.,
 ( 4, 2, 2, 2, 4 ),
 ( 0.000000000000000000, 0.002335515930058450207, 0.004671031860116900414, 0.007006547790175350621, 0.009342063720233800828 ),
 .UNSPECIFIED. ) ;
#6072 = TOROIDAL_SURFACE ( 'NONE', #5324, 7.924024642120688355, 1.000000000000000000 ) ;
#6073 = CARTESIAN_POINT ( 'NONE',  ( 0.000000000000000000, 21.75070940071359615, -33.00000000000012790 ) ) ;
#6074 = VERTEX_POINT ( 'NONE', #14622 ) ;
#6075 = CARTESIAN_POINT ( 'NONE',  ( 13.11297432109884653, -64.14571591460358491, 4.111538053172234974 ) ) ;
#6076 = EDGE_LOOP ( 'NONE', ( #2438, #2477, #14369, #9600 ) ) ;
#6077 = CARTESIAN_POINT ( 'NONE',  ( 29.69047892279256118, -53.28399145779480506, 4.141535524925028966 ) ) ;
#6078 = AXIS2_PLACEMENT_3D ( 'NONE', #9461, #1291, #3680 ) ;
#6079 = VERTEX_POINT ( 'NONE', #5250 ) ;
#6080 = AXIS2_PLACEMENT_3D ( 'NONE', #4552, #9410, #13946 ) ;
#6081 = CARTESIAN_POINT ( 'NONE',  ( 69.28051765693513175, -4.295678830383772961, 71.19766410831374515 ) ) ;
#6082 = FACE_OUTER_BOUND ( 'NONE', #11170, .T. ) ;
#6083 = ORIENTED_EDGE ( 'NONE', *, *, #11676, .T. ) ;
#6084 = DIRECTION ( 'NONE',  ( -0.000000000000000000, 0.000000000000000000, 1.000000000000000000 ) ) ;
#6085 = VECTOR ( 'NONE', #6044, 1000.000000000000000 ) ;
#6086 = DIRECTION ( 'NONE',  ( 0.000000000000000000, 0.000000000000000000, 1.000000000000000000 ) ) ;
#6087 = ORIENTED_EDGE ( 'NONE', *, *, #14483, .T. ) ;
#6088 = EDGE_CURVE ( 'NONE', #8692, #1292, #15072, .T. ) ;
#6089 = EDGE_CURVE ( 'NONE', #9571, #13132, #13113, .T. ) ;
#6090 = DIRECTION ( 'NONE',  ( 0.000000000000000000, 0.000000000000000000, 1.000000000000000000 ) ) ;
#6091 = DIRECTION ( 'NONE',  ( 1.000000000000000000, 0.000000000000000000, 0.000000000000000000 ) ) ;
#6092 = VECTOR ( 'NONE', #6676, 1000.000000000000000 ) ;
#6093 = DIRECTION ( 'NONE',  ( -0.000000000000000000, 1.000000000000000000, 1.445602896647339163E-16 ) ) ;
#6094 = ORIENTED_EDGE ( 'NONE', *, *, #5937, .F. ) ;
#6095 = CARTESIAN_POINT ( 'NONE',  ( 103.2469880950108063, 23.25070940071369208, 139.1143251403882459 ) ) ;
#6096 = CIRCLE ( 'NONE', #12725, 4.000000000000000000 ) ;
#6097 = ADVANCED_FACE ( 'NONE', ( #12472 ), #8773, .T. ) ;
#6098 = CIRCLE ( 'NONE', #7316, 0.7892041907098262810 ) ;
#6099 = ORIENTED_EDGE ( 'NONE', *, *, #6926, .T. ) ;
#6100 = CARTESIAN_POINT ( 'NONE',  ( 32.05794394608176390, -61.13769932686095387, -2.043477119560002997 ) ) ;
#6101 = DIRECTION ( 'NONE',  ( 1.000000000000000000, 0.000000000000000000, 0.000000000000000000 ) ) ;
#6102 = VERTEX_POINT ( 'NONE', #3015 ) ;
#6103 = CARTESIAN_POINT ( 'NONE',  ( -65.00000000000001421, -85.24929059928631148, 19.99999999999999645 ) ) ;
#6104 = DIRECTION ( 'NONE',  ( -0.8420378618367653223, -0.5394184268574524488, -0.000000000000000000 ) ) ;
#6105 = CIRCLE ( 'NONE', #3868, 1.000000000000000000 ) ;
#6106 = ADVANCED_FACE ( 'NONE', ( #12397 ), #8910, .T. ) ;
#6107 = CARTESIAN_POINT ( 'NONE',  ( -8.750650481006019277, 2.448077924947977380, -48.24789848114231461 ) ) ;
#6108 = CARTESIAN_POINT ( 'NONE',  ( 9.614235346878762911, -61.48375833289925652, 2.718831331508781979 ) ) ;
#6109 = AXIS2_PLACEMENT_3D ( 'NONE', #12054, #217, #9761 ) ;
#6110 = VECTOR ( 'NONE', #10667, 1000.000000000000000 ) ;
#6111 = LINE ( 'NONE', #5887, #13966 ) ;
#6112 = CARTESIAN_POINT ( 'NONE',  ( 53.04398595309534414, -1.224959495890951100, 62.84860122826521689 ) ) ;
#6113 = CARTESIAN_POINT ( 'NONE',  ( 33.12194698149885852, -54.49433873197092737, 2.092747212577964699 ) ) ;
#6114 = CARTESIAN_POINT ( 'NONE',  ( 31.85020396773706608, -53.04884725814062563, -2.499854452451645503 ) ) ;
#6115 = AXIS2_PLACEMENT_3D ( 'NONE', #6994, #978, #4684 ) ;
#6116 = CARTESIAN_POINT ( 'NONE',  ( 56.28732689558331259, 3.089731932287650640, 62.84860122826521689 ) ) ;
#6117 = VERTEX_POINT ( 'NONE', #11235 ) ;
#6118 =( LENGTH_UNIT ( ) NAMED_UNIT ( * ) SI_UNIT ( .MILLI., .METRE. ) );
#6119 = LINE ( 'NONE', #14198, #6213 ) ;
#6120 = AXIS2_PLACEMENT_3D ( 'NONE', #12905, #4740, #9595 ) ;
#6121 = CARTESIAN_POINT ( 'NONE',  ( 0.000000000000000000, 21.75070940071315562, 139.1143251403882459 ) ) ;
#6122 = DIRECTION ( 'NONE',  ( 0.000000000000000000, 1.000000000000000000, 0.000000000000000000 ) ) ;
#6123 = ORIENTED_EDGE ( 'NONE', *, *, #12887, .T. ) ;
#6124 = CARTESIAN_POINT ( 'NONE',  ( 76.44791115085612887, -7.901718459324428068, 76.13615421477460643 ) ) ;
#6125 = PLANE ( 'NONE',  #4206 ) ;
#6126 = EDGE_CURVE ( 'NONE', #10908, #1089, #2780, .T. ) ;
#6127 = CARTESIAN_POINT ( 'NONE',  ( 70.08269333764698672, -3.500995332129508864, 75.85600374239184873 ) ) ;
#6128 = DIRECTION ( 'NONE',  ( -0.5125013958363011657, -0.8586863916854879930, -0.000000000000000000 ) ) ;
#6129 = CARTESIAN_POINT ( 'NONE',  ( 32.36593770905977152, -54.69330887924043338, 3.128542914575001888 ) ) ;
#6130 = ADVANCED_FACE ( 'NONE', ( #3548 ), #3618, .T. ) ;
#6131 = ORIENTED_EDGE ( 'NONE', *, *, #10943, .T. ) ;
#6132 = ADVANCED_FACE ( 'NONE', ( #5631 ), #13777, .F. ) ;
#6133 = ADVANCED_FACE ( 'NONE', ( #8249 ), #10662, .T. ) ;
#6134 = CARTESIAN_POINT ( 'NONE',  ( 104.0000000000000426, 15.25070940071369563, -33.00000000000014211 ) ) ;
#6135 = ORIENTED_EDGE ( 'NONE', *, *, #7055, .T. ) ;
#6136 = LINE ( 'NONE', #13414, #13315 ) ;
#6137 = EDGE_LOOP ( 'NONE', ( #6525, #11863, #13007, #14651 ) ) ;
#6138 = ORIENTED_EDGE ( 'NONE', *, *, #15155, .F. ) ;
#6140 = VERTEX_POINT ( 'NONE', #11696 ) ;
#6139 = CARTESIAN_POINT ( 'NONE',  ( 64.66512137289342377, -11.59558090713824541, 75.55235509932406046 ) ) ;
#6141 = CARTESIAN_POINT ( 'NONE',  ( 58.00000000000000711, -2.249290599286309256, 47.51982618741348574 ) ) ;
#6142 = VECTOR ( 'NONE', #11249, 1000.000000000000000 ) ;
#6143 = EDGE_CURVE ( 'NONE', #3243, #6024, #3325, .T. ) ;
#6144 = CARTESIAN_POINT ( 'NONE',  ( 80.00000000000001421, -74.24929059928631148, 8.000000000000001776 ) ) ;
#6145 = VERTEX_POINT ( 'NONE', #12706 ) ;
#6146 = CARTESIAN_POINT ( 'NONE',  ( 8.749157052166545157, -56.32704560409226247, 2.799357392884345597 ) ) ;
#6147 = EDGE_CURVE ( 'NONE', #12382, #11210, #568, .T. ) ;
#6148 = PLANE ( 'NONE',  #8445 ) ;
#6149 = LINE ( 'NONE', #368, #2405 ) ;
#6150 = AXIS2_PLACEMENT_3D ( 'NONE', #8250, #3549, #14095 ) ;
#6151 = VECTOR ( 'NONE', #10039, 1000.000000000000000 ) ;
#6152 = ORIENTED_EDGE ( 'NONE', *, *, #13269, .F. ) ;
#6153 = ORIENTED_EDGE ( 'NONE', *, *, #3318, .F. ) ;
#6154 = EDGE_CURVE ( 'NONE', #3899, #5063, #3764, .T. ) ;
#6155 = DIRECTION ( 'NONE',  ( 1.000000000000000000, 8.270659117969274159E-16, 0.000000000000000000 ) ) ;
#6156 = ORIENTED_EDGE ( 'NONE', *, *, #7904, .F. ) ;
#6157 = DIRECTION ( 'NONE',  ( -0.8746197071345569451, 0.4848096202550666312, 0.000000000000000000 ) ) ;
#6158 = ORIENTED_EDGE ( 'NONE', *, *, #8013, .F. ) ;
#6159 = CARTESIAN_POINT ( 'NONE',  ( 23.47858629692699139, -53.24929059928630437, 6.492462156583989064 ) ) ;
#6160 = ORIENTED_EDGE ( 'NONE', *, *, #12, .F. ) ;
#6161 = LINE ( 'NONE', #6240, #5831 ) ;
#6162 = CARTESIAN_POINT ( 'NONE',  ( -11.45041300328984413, -9.336677115435668028, 48.21133583021728697 ) ) ;
#6163 = ORIENTED_EDGE ( 'NONE', *, *, #2016, .T. ) ;
#6164 = AXIS2_PLACEMENT_3D ( 'NONE', #887, #3285, #9057 ) ;
#6165 = DIRECTION ( 'NONE',  ( -0.8746197071345572782, 0.4848096202550659650, -0.000000000000000000 ) ) ;
#6166 = CARTESIAN_POINT ( 'NONE',  ( -21.66581936427349575, -2.249290599286303483, 50.50000000000012079 ) ) ;
#6167 = ORIENTED_EDGE ( 'NONE', *, *, #737, .T. ) ;
#6168 = LINE ( 'NONE', #10855, #3858 ) ;
#6169 = CARTESIAN_POINT ( 'NONE',  ( 66.38598137497019991, -11.47113225237460199, 71.19766410831374515 ) ) ;
#6170 = DIRECTION ( 'NONE',  ( 1.000000000000000000, 1.789942591005740441E-15, 0.000000000000000000 ) ) ;
#6171 = EDGE_CURVE ( 'NONE', #7961, #4611, #9434, .T. ) ;
#6172 = VERTEX_POINT ( 'NONE', #9088 ) ;
#6173 = DIRECTION ( 'NONE',  ( 0.000000000000000000, 0.000000000000000000, -1.000000000000000000 ) ) ;
#6174 = AXIS2_PLACEMENT_3D ( 'NONE', #1796, #1936, #6489 ) ;
#6175 = EDGE_CURVE ( 'NONE', #10987, #7187, #6769, .T. ) ;
#6176 = VERTEX_POINT ( 'NONE', #15014 ) ;
#6177 = ADVANCED_FACE ( 'NONE', ( #4461 ), #9171, .T. ) ;
#6178 = DIRECTION ( 'NONE',  ( 0.000000000000000000, 0.000000000000000000, 1.000000000000000000 ) ) ;
#6179 = FACE_OUTER_BOUND ( 'NONE', #9104, .T. ) ;
#6180 = ORIENTED_EDGE ( 'NONE', *, *, #2083, .T. ) ;
#6181 = VERTEX_POINT ( 'NONE', #3391 ) ;
#6182 = SHAPE_DEFINITION_REPRESENTATION ( #14687, #11972 ) ;
#6183 = CARTESIAN_POINT ( 'NONE',  ( 56.59738969056744651, 23.25070940071368852, 139.1143251403882459 ) ) ;
#6184 = LINE ( 'NONE', #10870, #5466 ) ;
#6185 = CARTESIAN_POINT ( 'NONE',  ( -8.563719136935748821, 2.126583234680710977, -48.00000000000012079 ) ) ;
#6186 = VECTOR ( 'NONE', #2913, 1000.000000000000000 ) ;
#6187 = CARTESIAN_POINT ( 'NONE',  ( 17.40655560130892354, -73.00063092933073960, 6.088059227066588086 ) ) ;
#6188 = CARTESIAN_POINT ( 'NONE',  ( 27.86173033120691045, -69.39711819508849544, 2.500000000000000000 ) ) ;
#6189 = DIRECTION ( 'NONE',  ( -0.8746197071345569451, 0.4848096202550666312, 0.000000000000000000 ) ) ;
#6190 = DIRECTION ( 'NONE',  ( -0.8208219420614839557, 0.4549890321264298820, 0.3453061251629756523 ) ) ;
#6191 = CARTESIAN_POINT ( 'NONE',  ( 31.45192786070105129, -52.79510901551774538, -2.616251790959260859 ) ) ;
#6192 = CIRCLE ( 'NONE', #9121, 4.000000000000000000 ) ;
#6193 =( BOUNDED_SURFACE ( )  B_SPLINE_SURFACE ( 3, 2, ( 
 ( #14934, #12707, #5713 ),
 ( #5551, #5632, #6770 ),
 ( #8171, #7009, #11697 ),
 ( #10321, #11622, #4625 ),
 ( #6932, #10401, #2079 ),
 ( #2156, #9247, #10 ),
 ( #13936, #9089, #6697 ),
 ( #2318, #9006, #6849 ),
 ( #4391, #4546, #8088 ),
 ( #920, #5790, #11536 ),
 ( #11385, #7938, #13709 ),
 ( #12552, #1155, #12791 ),
 ( #15096, #5873, #3392 ),
 ( #11457, #13778, #9320 ) ),
 .UNSPECIFIED., .F., .F., .F. ) 
 B_SPLINE_SURFACE_WITH_KNOTS ( ( 4, 2, 2, 2, 2, 2, 4 ),
 ( 3, 3 ),
 ( 0.2948322565876176915, 0.2981287057529254381, 0.3014251549182331846, 0.3080180532488486778, 0.3146109515794641709, 0.3179074007447718619, 0.3212038499100796085 ),
 ( 0.07447800286616089449, 1.000000000000000000 ),
 .UNSPECIFIED. ) 
 GEOMETRIC_REPRESENTATION_ITEM ( )  RATIONAL_B_SPLINE_SURFACE ( (
 ( 0.9996905063672956171, 0.9979222480410725460, 1.000000000000000000),
 ( 0.9996957508213679677, 0.9979574561150706957, 1.000000000000000000),
 ( 0.9997005874847066931, 0.9979899265301780398, 1.000000000000000000),
 ( 0.9997092625818482237, 0.9980481658545932167, 1.000000000000000000),
 ( 0.9997131045178146991, 0.9980739582752989891, 1.000000000000000000),
 ( 0.9997231512649209506, 0.9981414060230869856, 1.000000000000000000),
 ( 0.9997278760138150755, 0.9981731251127002880, 1.000000000000000000),
 ( 0.9997334421747796629, 0.9982104929310521291, 1.000000000000000000),
 ( 0.9997342833619660141, 0.9982161401500548870, 1.000000000000000000),
 ( 0.9997327054743884167, 0.9982055471728221718, 1.000000000000000000),
 ( 0.9997317056072283492, 0.9981988346730122919, 1.000000000000000000),
 ( 0.9997287795965361656, 0.9981791912173640924, 1.000000000000000000),
 ( 0.9997268671536081452, 0.9981663522390457066, 1.000000000000000000),
 ( 0.9997245403443034695, 0.9981507314569680878, 1.000000000000000000) ) ) 
 REPRESENTATION_ITEM ( '' )  SURFACE ( )  );
#6194 = PRESENTATION_LAYER_ASSIGNMENT (  '', '', ( #1004 ) ) ;
#6195 = EDGE_CURVE ( 'NONE', #11917, #604, #3279, .T. ) ;
#6196 = AXIS2_PLACEMENT_3D ( 'NONE', #10419, #2482, #4715 ) ;
#6197 = DIRECTION ( 'NONE',  ( 0.000000000000000000, -1.000000000000000000, 0.000000000000000000 ) ) ;
#6198 = ADVANCED_FACE ( 'NONE', ( #2235 ), #6931, .F. ) ;
#6199 = EDGE_LOOP ( 'NONE', ( #4752, #694, #300, #1851 ) ) ;
#6200 = FILL_AREA_STYLE_COLOUR ( '', #2747 ) ;
#6201 = CARTESIAN_POINT ( 'NONE',  ( -24.54316048551696028, -7.158540021523408292, -48.50000000000012079 ) ) ;
#6202 = LINE ( 'NONE', #11886, #12712 ) ;
#6203 = CARTESIAN_POINT ( 'NONE',  ( 69.46467306388282736, -2.354974971177655085, 75.74364963835485298 ) ) ;
#6204 = AXIS2_PLACEMENT_3D ( 'NONE', #4570, #10727, #1257 ) ;
#6205 = CARTESIAN_POINT ( 'NONE',  ( 98.40734512546775647, 0.000000000000000000, 139.1143251403882459 ) ) ;
#6206 = TOROIDAL_SURFACE ( 'NONE', #9885, 1.000000000000000000, 0.5000000000000000000 ) ;
#6207 = CARTESIAN_POINT ( 'NONE',  ( 65.52631879429515038, -10.90123334768769858, 71.19766412131004074 ) ) ;
#6208 = CARTESIAN_POINT ( 'NONE',  ( -3.999999999999976019, -69.24929059928631148, -32.99999999999998579 ) ) ;
#6209 = CARTESIAN_POINT ( 'NONE',  ( 27.86173033120691045, -69.39711819508849544, -3.619682905202609380 ) ) ;
#6210 = CARTESIAN_POINT ( 'NONE',  ( 33.59752155145360319, -57.15949554451621140, 1.814500213260170414 ) ) ;
#6211 = ORIENTED_EDGE ( 'NONE', *, *, #6003, .T. ) ;
#6212 = CYLINDRICAL_SURFACE ( 'NONE', #11794, 0.7892041907098262810 ) ;
#6213 = VECTOR ( 'NONE', #3655, 1000.000000000000000 ) ;
#6214 = VERTEX_POINT ( 'NONE', #7008 ) ;
#6215 = CARTESIAN_POINT ( 'NONE',  ( 66.92402464212069901, -2.249290599286308368, 47.51982618741348574 ) ) ;
#6216 = AXIS2_PLACEMENT_3D ( 'NONE', #13255, #7548, #536 ) ;
#6217 = ORIENTED_EDGE ( 'NONE', *, *, #5121, .T. ) ;
#6218 = ORIENTED_EDGE ( 'NONE', *, *, #6317, .T. ) ;
#6219 = LINE ( 'NONE', #1586, #4743 ) ;
#6220 = DIRECTION ( 'NONE',  ( 0.000000000000000000, -0.000000000000000000, -1.000000000000000000 ) ) ;
#6221 = CARTESIAN_POINT ( 'NONE',  ( 13.86173033120691223, -69.39711819508849544, 0.000000000000000000 ) ) ;
#6222 = VECTOR ( 'NONE', #12130, 1000.000000000000000 ) ;
#6223 = CARTESIAN_POINT ( 'NONE',  ( 8.094283469768480899, -56.86702399164115462, 2.513921072343785479 ) ) ;
#6224 = AXIS2_PLACEMENT_3D ( 'NONE', #4842, #14160, #8159 ) ;
#6225 = EDGE_CURVE ( 'NONE', #15020, #56, #336, .T. ) ;
#6226 = DIRECTION ( 'NONE',  ( -0.4543483311474731945, 0.8908241094534353754, 0.000000000000000000 ) ) ;
#6227 = EDGE_CURVE ( 'NONE', #14235, #9917, #8613, .T. ) ;
#6228 = FACE_OUTER_BOUND ( 'NONE', #4727, .T. ) ;
#6229 = VECTOR ( 'NONE', #12321, 1000.000000000000000 ) ;
#6230 = EDGE_CURVE ( 'NONE', #7295, #12140, #9682, .T. ) ;
#6231 = ORIENTED_EDGE ( 'NONE', *, *, #4688, .F. ) ;
#6232 = ORIENTED_EDGE ( 'NONE', *, *, #7752, .T. ) ;
#6233 = CARTESIAN_POINT ( 'NONE',  ( 71.80003071982790175, -14.47218880931180962, 72.19766410831374515 ) ) ;
#6234 = ORIENTED_EDGE ( 'NONE', *, *, #2568, .F. ) ;
#6235 = CARTESIAN_POINT ( 'NONE',  ( -24.96222495693456978, -7.431276100536581275, -57.50000000000012079 ) ) ;
#6236 = ORIENTED_EDGE ( 'NONE', *, *, #7826, .T. ) ;
#6237 = CARTESIAN_POINT ( 'NONE',  ( 29.48535251946016444, -62.76259148841293012, 3.786770376139651173 ) ) ;
#6238 = EDGE_LOOP ( 'NONE', ( #5883, #5392, #2223, #11902 ) ) ;
#6239 = VECTOR ( 'NONE', #8665, 1000.000000000000000 ) ;
#6240 = CARTESIAN_POINT ( 'NONE',  ( 88.00000000000001421, 10.75070940071369208, 84.20452624982236500 ) ) ;
#6241 = CARTESIAN_POINT ( 'NONE',  ( 65.80512781895316721, -6.575743597179691591, 82.40005259842790508 ) ) ;
#6242 = EDGE_LOOP ( 'NONE', ( #2228, #8600, #2337, #3617 ) ) ;
#6243 = AXIS2_PLACEMENT_3D ( 'NONE', #7312, #1544, #6021 ) ;
#6244 = EDGE_CURVE ( 'NONE', #1918, #8897, #3622, .T. ) ;
#6245 = EDGE_CURVE ( 'NONE', #3062, #10926, #5003, .T. ) ;
#6246 = CARTESIAN_POINT ( 'NONE',  ( 28.07070997989171701, -65.32322779889435083, -4.310009693574600398 ) ) ;
#6247 = EDGE_LOOP ( 'NONE', ( #2604, #7280, #184, #8906, #1066 ) ) ;
#6248 = DIRECTION ( 'NONE',  ( -0.000000000000000000, -1.000000000000000000, -1.682156097916903736E-15 ) ) ;
#6249 = CARTESIAN_POINT ( 'NONE',  ( 29.35555050496136431, -52.24929059928631148, 3.199931146564417350 ) ) ;
#6250 = DIRECTION ( 'NONE',  ( 0.000000000000000000, -1.000000000000000000, 0.000000000000000000 ) ) ;
#6251 = ORIENTED_EDGE ( 'NONE', *, *, #2741, .F. ) ;
#6252 = AXIS2_PLACEMENT_3D ( 'NONE', #11194, #14658, #12359 ) ;
#6253 = CARTESIAN_POINT ( 'NONE',  ( 65.13162939602317181, -11.91918766459985157, 73.19766410831374515 ) ) ;
#6254 = ORIENTED_EDGE ( 'NONE', *, *, #5859, .F. ) ;
#6255 = ORIENTED_EDGE ( 'NONE', *, *, #12109, .F. ) ;
#6256 = DIRECTION ( 'NONE',  ( -1.000000000000000000, -0.000000000000000000, -0.000000000000000000 ) ) ;
#6257 = ORIENTED_EDGE ( 'NONE', *, *, #14806, .T. ) ;
#6258 = DIRECTION ( 'NONE',  ( -1.000000000000000000, -8.673617379884035472E-17, 0.000000000000000000 ) ) ;
#6259 = DIRECTION ( 'NONE',  ( 1.000000000000000000, 0.000000000000000000, 0.000000000000000000 ) ) ;
#6260 = CARTESIAN_POINT ( 'NONE',  ( 7.981381109186949097, -53.52407281587392873, 2.732083153704975675 ) ) ;
#6261 = CARTESIAN_POINT ( 'NONE',  ( -11.54807159409575235, -9.445082653969818054, -48.38495513067856280 ) ) ;
#6262 = ADVANCED_FACE ( 'NONE', ( #10782 ), #13164, .T. ) ;
#6263 = CARTESIAN_POINT ( 'NONE',  ( 18.00000000000001066, 23.25070940071368497, -33.00000000000012790 ) ) ;
#6264 = CARTESIAN_POINT ( 'NONE',  ( 30.16905084671320481, -53.31390540393488919, -3.970772651015822774 ) ) ;
#6265 = DIRECTION ( 'NONE',  ( 1.000000000000000000, 0.000000000000000000, 0.000000000000000000 ) ) ;
#6266 = ORIENTED_EDGE ( 'NONE', *, *, #4268, .F. ) ;
#6267 = DIRECTION ( 'NONE',  ( 1.000000000000000000, 0.000000000000000000, 0.000000000000000000 ) ) ;
#6268 = CARTESIAN_POINT ( 'NONE',  ( 33.39134818684929940, -58.05408529505924520, -2.501672671492939148 ) ) ;
#6269 = DIRECTION ( 'NONE',  ( 0.8208219420614785156, -0.4549890321264269399, -0.3453061251629920836 ) ) ;
#6270 = CARTESIAN_POINT ( 'NONE',  ( 69.46454297106443221, -2.294433322023685662, 75.19766410831374515 ) ) ;
#6271 = CARTESIAN_POINT ( 'NONE',  ( 64.11356537587559501, -11.94785244090458498, 73.19766410831374515 ) ) ;
#6272 = CARTESIAN_POINT ( 'NONE',  ( 58.00000000000000711, -2.249290599286311032, 36.00000000000012079 ) ) ;
#6273 = EDGE_CURVE ( 'NONE', #4096, #3011, #4507, .T. ) ;
#6274 =( BOUNDED_SURFACE ( )  B_SPLINE_SURFACE ( 3, 2, ( 
 ( #12693, #6841, #13696 ),
 ( #1989, #10392, #10161 ),
 ( #681, #5388, #8924 ),
 ( #10084, #14846, #10231 ),
 ( #1840, #11527, #2147 ),
 ( #8996, #3152, #13618 ),
 ( #7852, #14922, #11299 ),
 ( #1916, #10310, #912 ) ),
 .UNSPECIFIED., .F., .F., .F. ) 
 B_SPLINE_SURFACE_WITH_KNOTS ( ( 4, 2, 2, 4 ),
 ( 3, 3 ),
 ( 0.000000000000000000, 0.001129222206655581574, 0.002258444413311163149, 0.004516888826622326297 ),
 ( 0.000000000000000000, 1.000000000000000000 ),
 .UNSPECIFIED. ) 
 GEOMETRIC_REPRESENTATION_ITEM ( )  RATIONAL_B_SPLINE_SURFACE ( (
 ( 1.000000000000000000, 0.7071067811864936159, 1.000000000000000000),
 ( 1.000000000000000000, 0.7608707698420138499, 1.000000000000000000),
 ( 1.000000000000000000, 0.8047257278452277784, 1.000000000000000000),
 ( 1.000000000000000000, 0.8783509392183566078, 1.000000000000000000),
 ( 1.000000000000000000, 0.9081758943102266057, 1.000000000000000000),
 ( 1.000000000000000000, 0.9781389570711758186, 1.000000000000000000),
 ( 1.000000000000000000, 0.9996704379314563793, 1.000000000000000000),
 ( 1.000000000000000000, 1.000000000000000000, 1.000000000000000000) ) ) 
 REPRESENTATION_ITEM ( '' )  SURFACE ( )  );
#6275 = FACE_OUTER_BOUND ( 'NONE', #727, .T. ) ;
#6276 = ORIENTED_EDGE ( 'NONE', *, *, #13173, .F. ) ;
#6277 = CARTESIAN_POINT ( 'NONE',  ( 23.72005712271144162, -60.79495753917990442, -6.390225278800149233 ) ) ;
#6278 = ORIENTED_EDGE ( 'NONE', *, *, #13891, .F. ) ;
#6279 = CARTESIAN_POINT ( 'NONE',  ( 20.86173033120691045, -87.24929059928631148, -3.999999999999999112 ) ) ;
#6280 = CARTESIAN_POINT ( 'NONE',  ( 24.62796245282055452, -85.24929059928631148, -1.347403282660978752 ) ) ;
#6281 = ORIENTED_EDGE ( 'NONE', *, *, #10684, .F. ) ;
#6282 = CYLINDRICAL_SURFACE ( 'NONE', #1282, 4.000000000000000000 ) ;
#6283 = CARTESIAN_POINT ( 'NONE',  ( -12.83418063572647760, -2.249290599286303927, -50.50000000000012079 ) ) ;
#6284 = CARTESIAN_POINT ( 'NONE',  ( -16.99999999999998579, -2.249290599286303927, 38.00000000000012079 ) ) ;
#6285 = EDGE_CURVE ( 'NONE', #3011, #4096, #7215, .T. ) ;
#6286 = ORIENTED_EDGE ( 'NONE', *, *, #10488, .T. ) ;
#6287 = VERTEX_POINT ( 'NONE', #1233 ) ;
#6288 = DIRECTION ( 'NONE',  ( -0.000000000000000000, -1.000000000000000000, -0.000000000000000000 ) ) ;
#6289 = DIRECTION ( 'NONE',  ( 0.000000000000000000, 1.000000000000000000, -0.000000000000000000 ) ) ;
#6290 = ORIENTED_EDGE ( 'NONE', *, *, #8077, .F. ) ;
#6291 = ORIENTED_EDGE ( 'NONE', *, *, #641, .F. ) ;
#6292 = DIRECTION ( 'NONE',  ( 0.000000000000000000, 1.000000000000000000, -0.000000000000000000 ) ) ;
#6293 = VERTEX_POINT ( 'NONE', #8401 ) ;
#6294 = DIRECTION ( 'NONE',  ( 0.3351302520855081735, 0.000000000000000000, 0.9421718071228324387 ) ) ;
#6295 = EDGE_LOOP ( 'NONE', ( #9250, #4836, #3919, #11710 ) ) ;
#6296 = CARTESIAN_POINT ( 'NONE',  ( 31.49298359385885249, -60.71197230342421136, 3.050751728647400629 ) ) ;
#6297 = VECTOR ( 'NONE', #14924, 1000.000000000000000 ) ;
#6298 = EDGE_CURVE ( 'NONE', #7044, #4976, #5749, .T. ) ;
#6299 = ORIENTED_EDGE ( 'NONE', *, *, #6245, .T. ) ;
#6300 = CARTESIAN_POINT ( 'NONE',  ( 72.12120841366726154, -14.65022051213588128, 75.25917400185288386 ) ) ;
#6301 = DIRECTION ( 'NONE',  ( 0.8656763553492622387, 0.5006040828731004311, -0.000000000000000000 ) ) ;
#6302 = ORIENTED_EDGE ( 'NONE', *, *, #9100, .F. ) ;
#6303 = CARTESIAN_POINT ( 'NONE',  ( 28.21768499689930465, -66.70046270226029606, -4.174231074483977011 ) ) ;
#6304 = ORIENTED_EDGE ( 'NONE', *, *, #2037, .F. ) ;
#6305 = AXIS2_PLACEMENT_3D ( 'NONE', #1915, #4294, #12460 ) ;
#6306 = AXIS2_PLACEMENT_3D ( 'NONE', #8255, #12951, #100 ) ;
#6307 = CARTESIAN_POINT ( 'NONE',  ( -28.95977857253363297, -8.587818791446675704, -48.50000000000012079 ) ) ;
#6308 = CYLINDRICAL_SURFACE ( 'NONE', #11559, 0.7892041907098261699 ) ;
#6309 = EDGE_CURVE ( 'NONE', #12860, #6626, #5079, .T. ) ;
#6310 = DIRECTION ( 'NONE',  ( -0.000000000000000000, -0.000000000000000000, -1.000000000000000000 ) ) ;
#6311 = ORIENTED_EDGE ( 'NONE', *, *, #6369, .T. ) ;
#6312 = CARTESIAN_POINT ( 'NONE',  ( 65.18587381434291217, -11.90669967090665793, 72.89354184684002291 ) ) ;
#6313 = EDGE_CURVE ( 'NONE', #12307, #11741, #6965, .T. ) ;
#6314 = ORIENTED_EDGE ( 'NONE', *, *, #14415, .F. ) ;
#6315 = AXIS2_PLACEMENT_3D ( 'NONE', #4082, #8567, #11096 ) ;
#6316 = ADVANCED_FACE ( 'NONE', ( #8480 ), #11887, .T. ) ;
#6317 = EDGE_CURVE ( 'NONE', #5708, #9131, #4853, .T. ) ;
#6318 = ORIENTED_EDGE ( 'NONE', *, *, #122, .F. ) ;
#6319 = CARTESIAN_POINT ( 'NONE',  ( 32.85032212349066327, -60.06401564186453612, -1.862089353234912315 ) ) ;
#6320 = AXIS2_PLACEMENT_3D ( 'NONE', #10213, #14985, #5368 ) ;
#6321 = CIRCLE ( 'NONE', #8296, 8.924024642120691908 ) ;
#6322 = ITEM_DEFINED_TRANSFORMATION ( 'NONE', 'NONE', #10994,  #6315 ) ;
#6323 = FACE_OUTER_BOUND ( 'NONE', #8577, .T. ) ;
#6324 = DIRECTION ( 'NONE',  ( 0.000000000000000000, -1.000000000000000000, 0.000000000000000000 ) ) ;
#6325 = EDGE_CURVE ( 'NONE', #10773, #7093, #8546, .T. ) ;
#6326 = CARTESIAN_POINT ( 'NONE',  ( -9.457494889590920550, -7.172893779636416056, -47.50000000000009237 ) ) ;
#6327 = CARTESIAN_POINT ( 'NONE',  ( 13.81473638797212011, -67.42803803082790637, 4.083598241712443233 ) ) ;
#6328 = CIRCLE ( 'NONE', #644, 8.924024642120691908 ) ;
#6329 = CARTESIAN_POINT ( 'NONE',  ( 130.4454129427046496, -1.749290599286305259, 13.14990448602692474 ) ) ;
#6330 = AXIS2_PLACEMENT_3D ( 'NONE', #10282, #9356, #2347 ) ;
#6331 = CARTESIAN_POINT ( 'NONE',  ( -16.99999999999998579, -2.249290599286303927, 57.50000000000012079 ) ) ;
#6332 = CARTESIAN_POINT ( 'NONE',  ( 10.23047706855496486, -60.71197230342421136, -3.050751728647411731 ) ) ;
#6333 = VECTOR ( 'NONE', #13403, 1000.000000000000000 ) ;
#6334 = CARTESIAN_POINT ( 'NONE',  ( -9.456839502978525047, 2.659958805273927140, 48.36906329404666849 ) ) ;
#6335 = ORIENTED_EDGE ( 'NONE', *, *, #13636, .T. ) ;
#6336 = FACE_OUTER_BOUND ( 'NONE', #5159, .T. ) ;
#6337 = VECTOR ( 'NONE', #6505, 1000.000000000000000 ) ;
#6338 = LINE ( 'NONE', #11030, #13210 ) ;
#6339 = AXIS2_PLACEMENT_3D ( 'NONE', #9453, #8589, #3745 ) ;
#6340 = EDGE_CURVE ( 'NONE', #6102, #5252, #11852, .T. ) ;
#6341 = VECTOR ( 'NONE', #10436, 1000.000000000000000 ) ;
#6342 = AXIS2_PLACEMENT_3D ( 'NONE', #8554, #9237, #6610 ) ;
#6343 = CARTESIAN_POINT ( 'NONE',  ( -80.00000000000001421, -74.24929059928631148, 32.99999999999999289 ) ) ;
#6344 = FACE_OUTER_BOUND ( 'NONE', #1253, .T. ) ;
#6345 = CARTESIAN_POINT ( 'NONE',  ( 27.61655672830269381, -69.39711819508849544, -4.282389493064020058 ) ) ;
#6346 = CARTESIAN_POINT ( 'NONE',  ( 62.80738265182633739, -4.914066317053381816, 86.40005259842790508 ) ) ;
#6347 = VECTOR ( 'NONE', #8688, 1000.000000000000000 ) ;
#6348 = ORIENTED_EDGE ( 'NONE', *, *, #13363, .F. ) ;
#6349 = DIRECTION ( 'NONE',  ( -0.000000000000000000, -0.000000000000000000, 1.000000000000000000 ) ) ;
#6350 = EDGE_LOOP ( 'NONE', ( #4161, #9699, #11896, #15121 ) ) ;
#6351 = CARTESIAN_POINT ( 'NONE',  ( 114.0000000000000284, 15.25070940071369563, 139.1143251403882459 ) ) ;
#6352 = DIRECTION ( 'NONE',  ( 1.000000000000000000, 0.000000000000000000, 0.000000000000000000 ) ) ;
#6353 = ORIENTED_EDGE ( 'NONE', *, *, #11242, .F. ) ;
#6355 = EDGE_LOOP ( 'NONE', ( #515, #12133, #6737 ) ) ;
#6354 = CARTESIAN_POINT ( 'NONE',  ( 53.34060950309435611, 1.272953934520814290, 62.84860122826521689 ) ) ;
#6356 = CARTESIAN_POINT ( 'NONE',  ( 109.8334623555409735, 21.75070940071366365, 33.00000000000012790 ) ) ;
#6357 = EDGE_CURVE ( 'NONE', #12008, #7657, #2695, .T. ) ;
#6358 = EDGE_CURVE ( 'NONE', #13865, #2105, #8921, .T. ) ;
#6359 = CARTESIAN_POINT ( 'NONE',  ( 80.00000000000001421, -74.24929059928631148, -32.99999999999999289 ) ) ;
#6360 = CARTESIAN_POINT ( 'NONE',  ( 0.5043391135745837195, 0.8906624217387615339, 58.00000000000012079 ) ) ;
#6361 = CARTESIAN_POINT ( 'NONE',  ( -16.99999999999998579, -2.249290599286303927, 33.00000000000012790 ) ) ;
#6362 = CARTESIAN_POINT ( 'NONE',  ( 54.30726695196912601, -6.397170215889376621, 48.51982618741349285 ) ) ;
#6363 = ORIENTED_EDGE ( 'NONE', *, *, #7910, .F. ) ;
#6364 = DIRECTION ( 'NONE',  ( 0.000000000000000000, -0.000000000000000000, -1.000000000000000000 ) ) ;
#6365 = ORIENTED_EDGE ( 'NONE', *, *, #2058, .F. ) ;
#6366 = CARTESIAN_POINT ( 'NONE',  ( -23.68126483017411488, 3.790603994468874749, 47.74939190649463683 ) ) ;
#6367 = ORIENTED_EDGE ( 'NONE', *, *, #11228, .T. ) ;
#6368 = DIRECTION ( 'NONE',  ( 0.000000000000000000, 1.000000000000000000, 2.312964634635740689E-15 ) ) ;
#6369 = EDGE_CURVE ( 'NONE', #14121, #5503, #2295, .T. ) ;
#6370 = EDGE_CURVE ( 'NONE', #11451, #13978, #12124, .T. ) ;
#6371 = EDGE_LOOP ( 'NONE', ( #14664, #6094, #15037, #4369 ) ) ;
#6372 = PRODUCT_DEFINITION ( 'UNKNOWN', '', #14446, #9213 ) ;
#6373 = CARTESIAN_POINT ( 'NONE',  ( 65.00000000000001421, -85.24929059928629727, -17.47499999999999787 ) ) ;
#6374 = LINE ( 'NONE', #5218, #9407 ) ;
#6375 = ORIENTED_EDGE ( 'NONE', *, *, #4142, .T. ) ;
#6376 = VERTEX_POINT ( 'NONE', #14323 ) ;
#6377 = CIRCLE ( 'NONE', #9326, 4.000000000000003553 ) ;
#6378=STYLED_ITEM('',(#15258),#9466);
#6379 = LINE ( 'NONE', #3837, #7588 ) ;
#6380 = DIRECTION ( 'NONE',  ( -0.8746197071345570562, 0.4848096202550665756, 0.000000000000000000 ) ) ;
#6381 = FACE_OUTER_BOUND ( 'NONE', #5359, .T. ) ;
#6382 = ORIENTED_EDGE ( 'NONE', *, *, #13432, .F. ) ;
#6383 = FACE_OUTER_BOUND ( 'NONE', #4079, .T. ) ;
#6384 = EDGE_LOOP ( 'NONE', ( #3018, #13555, #8675, #14447 ) ) ;
#6385 = ORIENTED_EDGE ( 'NONE', *, *, #6585, .T. ) ;
#6386 = CARTESIAN_POINT ( 'NONE',  ( 27.62809333727740224, -69.39711819508848123, 4.287213148048561351 ) ) ;
#6387 = AXIS2_PLACEMENT_3D ( 'NONE', #7110, #4879, #1255 ) ;
#6388 = SHAPE_DEFINITION_REPRESENTATION ( #4375, #13539 ) ;
#6389 = LINE ( 'NONE', #7400, #2410 ) ;
#6390 = EDGE_CURVE ( 'NONE', #12128, #14607, #2837, .T. ) ;
#6391 = CARTESIAN_POINT ( 'NONE',  ( 58.00000000000000711, -2.249290599286309256, 72.19766410831374515 ) ) ;
#6392 = FACE_OUTER_BOUND ( 'NONE', #10427, .T. ) ;
#6393 = PLANE ( 'NONE',  #558 ) ;
#6394 = CARTESIAN_POINT ( 'NONE',  ( -8.537170960192327129, 2.067018546614582508, -58.00000000000012079 ) ) ;
#6395 = CARTESIAN_POINT ( 'NONE',  ( 88.00000000000000000, 23.25070940071369208, -33.00000000000012790 ) ) ;
#6396 = PRESENTATION_LAYER_ASSIGNMENT (  '', '', ( #13046 ) ) ;
#6397 = CARTESIAN_POINT ( 'NONE',  ( -9.456839514482961562, 2.659958822950721835, 48.50000000000012079 ) ) ;
#6398 = EDGE_CURVE ( 'NONE', #3110, #5708, #8832, .T. ) ;
#6399 = DIRECTION ( 'NONE',  ( 0.000000000000000000, 0.000000000000000000, 1.000000000000000000 ) ) ;
#6400 = ORIENTED_EDGE ( 'NONE', *, *, #10279, .F. ) ;
#6401 = CARTESIAN_POINT ( 'NONE',  ( 58.00000000000000711, -2.249290599286311032, -33.00000000000012790 ) ) ;
#6402 = CYLINDRICAL_SURFACE ( 'NONE', #7363, 31.00000000000000000 ) ;
#6403 = TOROIDAL_SURFACE ( 'NONE', #13052, 4.165819364273509962, 0.5000000000000000000 ) ;
#6404 = CARTESIAN_POINT ( 'NONE',  ( 62.80738265182633739, -4.914066317053381816, 82.40005259842790508 ) ) ;
#6405 = EDGE_LOOP ( 'NONE', ( #7562, #1649, #13675, #1595 ) ) ;
#6406 = CARTESIAN_POINT ( 'NONE',  ( 8.821484763567294607, -57.33450387999030795, 2.749014434309869248 ) ) ;
#6407 = CARTESIAN_POINT ( 'NONE',  ( -24.12409601409935078, -6.885803942510236197, 57.50000000000012079 ) ) ;
#6408 = EDGE_CURVE ( 'NONE', #5046, #10853, #1802, .T. ) ;
#6409 = EDGE_CURVE ( 'NONE', #9304, #11686, #5495, .T. ) ;
#6410 = VECTOR ( 'NONE', #7376, 999.9999999999998863 ) ;
#6411 = DIRECTION ( 'NONE',  ( 1.000000000000000000, 0.000000000000000000, 0.000000000000000000 ) ) ;
#6412 = CARTESIAN_POINT ( 'NONE',  ( 58.00000000000000711, -2.249290599286309256, 48.51982618741349285 ) ) ;
#6413 = CARTESIAN_POINT ( 'NONE',  ( 71.94624495291445498, -14.55323668216481536, 72.13615421477459222 ) ) ;
#6414 = AXIS2_PLACEMENT_3D ( 'NONE', #7310, #8248, #2389 ) ;
#6415 = ORIENTED_EDGE ( 'NONE', *, *, #12965, .F. ) ;
#6416 = DIRECTION ( 'NONE',  ( 0.8746197071345569451, -0.4848096202550666312, 0.000000000000000000 ) ) ;
#6417 = ORIENTED_EDGE ( 'NONE', *, *, #3628, .T. ) ;
#6418 = DIRECTION ( 'NONE',  ( -0.000000000000000000, 1.000000000000000000, -0.000000000000000000 ) ) ;
#6419 = FACE_OUTER_BOUND ( 'NONE', #3885, .T. ) ;
#6420 = ORIENTED_EDGE ( 'NONE', *, *, #10684, .T. ) ;
#6421 = CIRCLE ( 'NONE', #15030, 0.7892041907098250597 ) ;
#6423 = EDGE_LOOP ( 'NONE', ( #5501, #15086, #11912, #9333 ) ) ;
#6422 = DIRECTION ( 'NONE',  ( 1.000000000000000000, 0.000000000000000000, 0.000000000000000000 ) ) ;
#6424 = DIRECTION ( 'NONE',  ( 0.000000000000000000, -1.000000000000000000, -1.445602896647339410E-16 ) ) ;
#6425 = AXIS2_PLACEMENT_3D ( 'NONE', #1458, #9312, #7003 ) ;
#6426 = AXIS2_PLACEMENT_3D ( 'NONE', #4406, #9110, #3258 ) ;
#6427 = CARTESIAN_POINT ( 'NONE',  ( 11.46205536272528036, -61.79747627231518692, 3.500139319475375821 ) ) ;
#6428 = CARTESIAN_POINT ( 'NONE',  ( 9.936896301974771362, -54.06072418659005763, 3.368302239731210790 ) ) ;
#6429 = CARTESIAN_POINT ( 'NONE',  ( 26.26264421955999495, -69.39711819508849544, 5.076148092048932803 ) ) ;
#6430 = MECHANICAL_DESIGN_GEOMETRIC_PRESENTATION_REPRESENTATION (  '', ( #11103 ), #8173 ) ;
#6431 = AXIS2_PLACEMENT_3D ( 'NONE', #2962, #4176, #5272 ) ;
#6432 = ADVANCED_FACE ( 'NONE', ( #8755 ), #6456, .F. ) ;
#6433 = LINE ( 'NONE', #8892, #6337 ) ;
#6434 = AXIS2_PLACEMENT_3D ( 'NONE', #4777, #12938, #14164 ) ;
#6435 = VERTEX_POINT ( 'NONE', #5456 ) ;
#6436 = CARTESIAN_POINT ( 'NONE',  ( 8.848596353267785375, -60.00492685494598533, 2.531405393172750706 ) ) ;
#6437 = ORIENTED_EDGE ( 'NONE', *, *, #1419, .F. ) ;
#6438 = CARTESIAN_POINT ( 'NONE',  ( 66.38598137497019991, -11.47113225237460910, 72.19766410831374515 ) ) ;
#6439 = ORIENTED_EDGE ( 'NONE', *, *, #11630, .F. ) ;
#6440 = CARTESIAN_POINT ( 'NONE',  ( 27.32034923808841498, -68.64054039872955570, 4.542265185094224833 ) ) ;
#6441 = DIRECTION ( 'NONE',  ( 0.000000000000000000, 0.000000000000000000, 1.000000000000000000 ) ) ;
#6442 = VECTOR ( 'NONE', #9938, 1000.000000000000000 ) ;
#6443 = FACE_OUTER_BOUND ( 'NONE', #1190, .T. ) ;
#6444 = CARTESIAN_POINT ( 'NONE',  ( -5.290523468902621929, 4.522075770548486418, -48.50000000000012079 ) ) ;
#6445 = ORIENTED_EDGE ( 'NONE', *, *, #4035, .T. ) ;
#6446 = CIRCLE ( 'NONE', #7645, 0.5000000000000000000 ) ;
#6447 = VECTOR ( 'NONE', #10567, 1000.000000000000000 ) ;
#6448 = CARTESIAN_POINT ( 'NONE',  ( 31.27094208185658530, -61.76394201828218655, -3.065891788248765515 ) ) ;
#6449 = ORIENTED_EDGE ( 'NONE', *, *, #10446, .F. ) ;
#6450 = CIRCLE ( 'NONE', #5226, 0.9999999999999996669 ) ;
#6451 = DIRECTION ( 'NONE',  ( -0.000000000000000000, 0.000000000000000000, -1.000000000000000000 ) ) ;
#6452 = DIRECTION ( 'NONE',  ( 1.000000000000000000, 0.000000000000000000, 0.000000000000000000 ) ) ;
#6453 = DIRECTION ( 'NONE',  ( 1.000000000000000000, 0.000000000000000000, 0.000000000000000000 ) ) ;
#6454 = EDGE_CURVE ( 'NONE', #14376, #8736, #13380, .T. ) ;
#6455 = EDGE_CURVE ( 'NONE', #14153, #4443, #11150, .T. ) ;
#6456 = PLANE ( 'NONE',  #2045 ) ;
#6457 = ORIENTED_EDGE ( 'NONE', *, *, #311, .F. ) ;
#6458 = VECTOR ( 'NONE', #7811, 1000.000000000000000 ) ;
#6459 = DIRECTION ( 'NONE',  ( 0.000000000000000000, -0.000000000000000000, 1.000000000000000000 ) ) ;
#6460 = VERTEX_POINT ( 'NONE', #600 ) ;
#6461 = ORIENTED_EDGE ( 'NONE', *, *, #1829, .T. ) ;
#6462 = AXIS2_PLACEMENT_3D ( 'NONE', #11978, #6288, #1363 ) ;
#6463 = EDGE_LOOP ( 'NONE', ( #5791, #4854, #11443, #13783 ) ) ;
#6464 = AXIS2_PLACEMENT_3D ( 'NONE', #12196, #12132, #363 ) ;
#6465 = DIRECTION ( 'NONE',  ( -0.000000000000000000, 0.000000000000000000, -1.000000000000000000 ) ) ;
#6466 = DIRECTION ( 'NONE',  ( -0.000000000000000000, -0.000000000000000000, -1.000000000000000000 ) ) ;
#6467 = DIRECTION ( 'NONE',  ( 0.8746197071345571672, -0.4848096202550660205, 0.000000000000000000 ) ) ;
#6468 = CARTESIAN_POINT ( 'NONE',  ( 58.00000000000000711, -2.249290599286309256, 71.19766410831374515 ) ) ;
#6469 = ORIENTED_EDGE ( 'NONE', *, *, #14309, .T. ) ;
#6470 = ADVANCED_FACE ( 'NONE', ( #14755 ), #13528, .F. ) ;
#6471 = DIRECTION ( 'NONE',  ( 0.000000000000000000, 0.000000000000000000, 1.000000000000000000 ) ) ;
#6472 = AXIS2_PLACEMENT_3D ( 'NONE', #11265, #8730, #5432 ) ;
#6473 = CARTESIAN_POINT ( 'NONE',  ( 63.55116547662792215, -2.088839582009629936, 54.56811043785582882 ) ) ;
#6474 = DIRECTION ( 'NONE',  ( -0.000000000000000000, 0.000000000000000000, -1.000000000000000000 ) ) ;
#6475 = AXIS2_PLACEMENT_3D ( 'NONE', #9400, #3470, #2317 ) ;
#6476 = CARTESIAN_POINT ( 'NONE',  ( 59.00001739350650354, 10.75070940071368852, -33.00000000000012790 ) ) ;
#6477 = CARTESIAN_POINT ( 'NONE',  ( 12.23810814295215721, -62.76259148841472069, -3.786770376138867356 ) ) ;
#6478 = ORIENTED_EDGE ( 'NONE', *, *, #10794, .F. ) ;
#6479 = CARTESIAN_POINT ( 'NONE',  ( 32.93458379808025427, -56.07566194134380311, 2.832314198475984757 ) ) ;
#6480 = CARTESIAN_POINT ( 'NONE',  ( -8.750650481006019277, 2.448077924947977380, 48.24789848114231461 ) ) ;
#6481 = ORIENTED_EDGE ( 'NONE', *, *, #1968, .T. ) ;
#6482 = DIRECTION ( 'NONE',  ( 0.000000000000000000, 1.000000000000000000, 0.000000000000000000 ) ) ;
#6483 = CARTESIAN_POINT ( 'NONE',  ( 8.091875466796944139, -56.52532528994184702, -1.842181053809134994 ) ) ;
#6484 = CARTESIAN_POINT ( 'NONE',  ( 100.1541764164548880, 21.75070940071359615, -33.00000000000012790 ) ) ;
#6485 = ORIENTED_EDGE ( 'NONE', *, *, #9661, .F. ) ;
#6486 = LINE ( 'NONE', #626, #11426 ) ;
#6487 = EDGE_CURVE ( 'NONE', #9446, #11132, #12381, .T. ) ;
#6488 = CYLINDRICAL_SURFACE ( 'NONE', #5147, 0.7892041907098262810 ) ;
#6489 = DIRECTION ( 'NONE',  ( 0.8420378618367644341, 0.5394184268574535590, 0.000000000000000000 ) ) ;
#6490 = CARTESIAN_POINT ( 'NONE',  ( -25.01741698508091005, -6.338425579613558014, -47.50000000000012079 ) ) ;
#6491 = ORIENTED_EDGE ( 'NONE', *, *, #292, .F. ) ;
#6492 = CARTESIAN_POINT ( 'NONE',  ( 23.93808696748097375, -66.03679020159736979, -6.288305159851794279 ) ) ;
#6493 = ORIENTED_EDGE ( 'NONE', *, *, #11876, .F. ) ;
#6494 = EDGE_CURVE ( 'NONE', #8958, #13411, #11067, .T. ) ;
#6495 = CARTESIAN_POINT ( 'NONE',  ( -21.66581936427349575, -2.249290599286303483, 50.00000000000012079 ) ) ;
#6496 = DIRECTION ( 'NONE',  ( -0.000000000000000000, -0.000000000000000000, -1.000000000000000000 ) ) ;
#6497 = ADVANCED_FACE ( 'NONE', ( #8686 ), #4056, .T. ) ;
#6498 = ORIENTED_EDGE ( 'NONE', *, *, #2503, .F. ) ;
#6499 = CARTESIAN_POINT ( 'NONE',  ( 56.59738969056744651, 21.75070940071329417, 139.1143251403882459 ) ) ;
#6500 = LINE ( 'NONE', #577, #2122 ) ;
#6501 = CARTESIAN_POINT ( 'NONE',  ( 11.98773490706794753, -63.50313342087472535, 3.632148419028808473 ) ) ;
#6502 = EDGE_CURVE ( 'NONE', #965, #8509, #6713, .T. ) ;
#6503 = CARTESIAN_POINT ( 'NONE',  ( 108.0866310645538562, 0.000000000000000000, 139.1143251403882459 ) ) ;
#6504 = LINE ( 'NONE', #11125, #14355 ) ;
#6505 = DIRECTION ( 'NONE',  ( -0.000000000000000000, -0.000000000000000000, -1.000000000000000000 ) ) ;
#6506 = VERTEX_POINT ( 'NONE', #11215 ) ;
#6507 = CARTESIAN_POINT ( 'NONE',  ( 8.599030766203952680, -59.21224831720009263, 1.832439066040497444 ) ) ;
#6508 = ORIENTED_EDGE ( 'NONE', *, *, #5564, .T. ) ;
#6509 = DIRECTION ( 'NONE',  ( -0.000000000000000000, 1.000000000000000000, -0.000000000000000000 ) ) ;
#6510 = ORIENTED_EDGE ( 'NONE', *, *, #4385, .T. ) ;
#6511 = CARTESIAN_POINT ( 'NONE',  ( 27.85761975137827662, -68.67486713609795856, 3.656664647229231235 ) ) ;
#6512 = CARTESIAN_POINT ( 'NONE',  ( -9.037775043065350289, 2.932694901963889933, -48.50000000000012079 ) ) ;
#6513 = DIRECTION ( 'NONE',  ( 0.000000000000000000, 0.000000000000000000, 1.000000000000000000 ) ) ;
#6514 = LINE ( 'NONE', #9143, #818 ) ;
#6515 = ORIENTED_EDGE ( 'NONE', *, *, #4967, .T. ) ;
#6516 = ADVANCED_FACE ( 'NONE', ( #6381 ), #744, .T. ) ;
#6517 = CARTESIAN_POINT ( 'NONE',  ( -16.99999999999998579, -2.249290599286305703, -32.99999999999987921 ) ) ;
#6518 = EDGE_LOOP ( 'NONE', ( #3101, #14958, #12191, #14628, #3459, #6536, #10674, #8089, #11315, #14858, #12534, #12922, #2873, #3373, #94, #11910, #4766, #7516, #10182, #5598, #9603, #15081, #14539, #4100, #2472, #1137, #11464, #4687, #7703, #9324, #7694, #12186, #9765, #2960, #6156, #12494, #2627, #6449, #13989, #4977, #13691, #1394, #15153, #1972, #6123, #3458, #6938, #9752, #5651, #7572, #5500, #12298, #8464, #8875, #5676, #3824, #8310, #9402, #13614, #4713, #5125, #14457, #6251, #6236, #14598, #14100 ) ) ;
#6519 = DIRECTION ( 'NONE',  ( 0.000000000000000000, -1.000000000000000000, 0.000000000000000000 ) ) ;
#6520 = DIRECTION ( 'NONE',  ( -0.000000000000000000, -0.000000000000000000, -1.000000000000000000 ) ) ;
#6521 = CARTESIAN_POINT ( 'NONE',  ( -16.99999999999998579, -2.249290599286305703, 33.00000000000012790 ) ) ;
#6522 = VERTEX_POINT ( 'NONE', #3070 ) ;
#6523 = AXIS2_PLACEMENT_3D ( 'NONE', #8789, #13484, #12334 ) ;
#6524 = CARTESIAN_POINT ( 'NONE',  ( -16.99999999999998579, -2.249290599286303927, 58.00000000000012079 ) ) ;
#6525 = ORIENTED_EDGE ( 'NONE', *, *, #14073, .F. ) ;
#6526 = ORIENTED_EDGE ( 'NONE', *, *, #1346, .F. ) ;
#6527 = ORIENTED_EDGE ( 'NONE', *, *, #2123, .T. ) ;
#6528 = FILL_AREA_STYLE ('',( #14691 ) ) ;
#6529 = ITEM_DEFINED_TRANSFORMATION ( 'NONE', 'NONE', #4342,  #6315 ) ;
#6530 = DIRECTION ( 'NONE',  ( 0.000000000000000000, 0.000000000000000000, 1.000000000000000000 ) ) ;
#6531 = DIRECTION ( 'NONE',  ( 1.156482317317870492E-16, -1.000000000000000000, 0.000000000000000000 ) ) ;
#6532 = EDGE_CURVE ( 'NONE', #5487, #9598, #7470, .T. ) ;
#6533 = EDGE_CURVE ( 'NONE', #5927, #1834, #5229, .T. ) ;
#6534 = CARTESIAN_POINT ( 'NONE',  ( 53.19261734817368392, 0.4154851184807644149, 86.40005259842790508 ) ) ;
#6535 = CIRCLE ( 'NONE', #12436, 0.9999999999999996669 ) ;
#6536 = ORIENTED_EDGE ( 'NONE', *, *, #2501, .T. ) ;
#6537 = DIRECTION ( 'NONE',  ( -1.000000000000000000, 0.000000000000000000, 0.000000000000000000 ) ) ;
#6538 = CARTESIAN_POINT ( 'NONE',  ( -16.99999999999998579, -2.249290599286303927, 50.00000000000012079 ) ) ;
#6539 = PLANE ( 'NONE',  #962 ) ;
#6540 = EDGE_LOOP ( 'NONE', ( #6763, #3198, #14910, #1658 ) ) ;
#6541 = DIRECTION ( 'NONE',  ( -0.5006040828730242698, 0.8656763553493063146, 0.000000000000000000 ) ) ;
#6542 = AXIS2_PLACEMENT_3D ( 'NONE', #9310, #3686, #232 ) ;
#6543 = AXIS2_PLACEMENT_3D ( 'NONE', #6964, #14967, #12582 ) ;
#6544 = CARTESIAN_POINT ( 'NONE',  ( 53.34060950309435611, 1.272953934520814734, 60.61639468829817190 ) ) ;
#6545 = EDGE_LOOP ( 'NONE', ( #7428, #11083, #2120, #5417 ) ) ;
#6546 =( NAMED_UNIT ( * ) PLANE_ANGLE_UNIT ( ) SI_UNIT ( $, .RADIAN. ) );
#6547 = CARTESIAN_POINT ( 'NONE',  ( 80.00000000000001421, -74.24929059928631148, -4.000000000000000000 ) ) ;
#6548 = EDGE_CURVE ( 'NONE', #11623, #6609, #5301, .T. ) ;
#6549 = ADVANCED_FACE ( 'NONE', ( #9997 ), #953, .F. ) ;
#6550 = CARTESIAN_POINT ( 'NONE',  ( -16.99999999999998579, -2.249290599286303927, 57.50000000000012079 ) ) ;
#6551 = ORIENTED_EDGE ( 'NONE', *, *, #6245, .F. ) ;
#6552 = AXIS2_PLACEMENT_3D ( 'NONE', #903, #5537, #5693 ) ;
#6553 = CIRCLE ( 'NONE', #12200, 2.000000000000001776 ) ;
#6554 = CARTESIAN_POINT ( 'NONE',  ( 72.26742264675378635, -14.73126838498887281, 75.19766410831374515 ) ) ;
#6555 = AXIS2_PLACEMENT_3D ( 'NONE', #2718, #11097, #7419 ) ;
#6556 = CARTESIAN_POINT ( 'NONE',  ( 12.48148056143272733, -64.22824823034754615, 3.135769320951038441 ) ) ;
#6557 = LINE ( 'NONE', #13722, #10563 ) ;
#6558 = CARTESIAN_POINT ( 'NONE',  ( -26.99999999999998934, -2.249290599286303927, 38.00000000000012079 ) ) ;
#6559 = VECTOR ( 'NONE', #9458, 1000.000000000000000 ) ;
#6560 = ORIENTED_EDGE ( 'NONE', *, *, #8948, .F. ) ;
#6561 = FACE_OUTER_BOUND ( 'NONE', #4858, .T. ) ;
#6562 = CIRCLE ( 'NONE', #14449, 4.000000000000003553 ) ;
#6563 = VERTEX_POINT ( 'NONE', #13760 ) ;
#6564 = DIRECTION ( 'NONE',  ( -1.000000000000000000, -1.156482317317870492E-16, 0.000000000000000000 ) ) ;
#6565 = CARTESIAN_POINT ( 'NONE',  ( 32.39917484285220439, 23.25070940071368852, 33.00000000000012790 ) ) ;
#6566 = CIRCLE ( 'NONE', #10757, 6.484807146443463566 ) ;
#6567 = VERTEX_POINT ( 'NONE', #4526 ) ;
#6568 = LINE ( 'NONE', #10118, #12113 ) ;
#6569 = FACE_BOUND ( 'NONE', #14058, .T. ) ;
#6570 = ORIENTED_EDGE ( 'NONE', *, *, #10935, .T. ) ;
#6571 = CARTESIAN_POINT ( 'NONE',  ( 76.61154307727187529, -6.849067049365817006, 73.07464432123545350 ) ) ;
#6572 = EDGE_CURVE ( 'NONE', #4603, #341, #14994, .T. ) ;
#6573 = AXIS2_PLACEMENT_3D ( 'NONE', #2473, #9640, #1547 ) ;
#6574 = CARTESIAN_POINT ( 'NONE',  ( 71.64423341085262109, -14.38582895075278500, 73.19766410831374515 ) ) ;
#6575 = CARTESIAN_POINT ( 'NONE',  ( 31.74060458544689922, -52.97269888719504394, -2.532182285388751897 ) ) ;
#6576 = ADVANCED_FACE ( 'NONE', ( #11435 ), #1129, .T. ) ;
#6577 = PRODUCT ( 'Locking Handle', 'Locking Handle', '', ( #9648 ) ) ;
#6578 = VECTOR ( 'NONE', #9731, 1000.000000000000000 ) ;
#6579 = EDGE_CURVE ( 'NONE', #6582, #6752, #7708, .T. ) ;
#6580 = DIRECTION ( 'NONE',  ( -0.000000000000000000, 1.000000000000000000, 0.000000000000000000 ) ) ;
#6581 = CARTESIAN_POINT ( 'NONE',  ( 80.00000000000001421, -72.24929059928631148, 32.99999999999999289 ) ) ;
#6582 = VERTEX_POINT ( 'NONE', #1061 ) ;
#6583 = DIRECTION ( 'NONE',  ( -1.000000000000000000, 0.000000000000000000, 0.000000000000000000 ) ) ;
#6584 = ORIENTED_EDGE ( 'NONE', *, *, #8496, .F. ) ;
#6585 = EDGE_CURVE ( 'NONE', #12155, #298, #12853, .T. ) ;
#6586 = DIRECTION ( 'NONE',  ( 0.000000000000000000, 0.000000000000000000, 1.000000000000000000 ) ) ;
#6587 = ORIENTED_EDGE ( 'NONE', *, *, #7287, .F. ) ;
#6588 = DIRECTION ( 'NONE',  ( 0.8746197071345570562, -0.4848096202550662981, 0.000000000000000000 ) ) ;
#6589 = EDGE_CURVE ( 'NONE', #4392, #12856, #5176, .T. ) ;
#6590 = DIRECTION ( 'NONE',  ( 1.000000000000000000, 0.000000000000000000, 0.000000000000000000 ) ) ;
#6591 = CYLINDRICAL_SURFACE ( 'NONE', #8762, 0.7892041907098262810 ) ;
#6592 = DIRECTION ( 'NONE',  ( 0.000000000000000000, 0.000000000000000000, 1.000000000000000000 ) ) ;
#6593 = EDGE_LOOP ( 'NONE', ( #8805, #14552, #12286, #10579 ) ) ;
#6594 = EDGE_CURVE ( 'NONE', #4084, #13411, #4602, .T. ) ;
#6595 = DIRECTION ( 'NONE',  ( 0.000000000000000000, 0.000000000000000000, 1.000000000000000000 ) ) ;
#6596 = VERTEX_POINT ( 'NONE', #11600 ) ;
#6597 = ADVANCED_FACE ( 'NONE', ( #3372 ), #13993, .F. ) ;
#6598 = EDGE_CURVE ( 'NONE', #2975, #3404, #4681, .T. ) ;
#6599 = CARTESIAN_POINT ( 'NONE',  ( 62.67308791069655882, 29.52935533987996664, -33.00000000000013500 ) ) ;
#6600 = CARTESIAN_POINT ( 'NONE',  ( 80.18290120114222930, 25.52935533987996664, -33.00000000000014211 ) ) ;
#6601 = CYLINDRICAL_SURFACE ( 'NONE', #14097, 2.499999999999995115 ) ;
#6602 = CARTESIAN_POINT ( 'NONE',  ( 76.00751999314820750, -6.514251586541772276, 71.19766410831374515 ) ) ;
#6603 = ORIENTED_EDGE ( 'NONE', *, *, #74, .F. ) ;
#6604 = LINE ( 'NONE', #2999, #6347 ) ;
#6605 = EDGE_CURVE ( 'NONE', #11544, #1585, #10011, .T. ) ;
#6606 = ORIENTED_EDGE ( 'NONE', *, *, #5328, .T. ) ;
#6607 = CARTESIAN_POINT ( 'NONE',  ( 64.90552635791956959, 12.46743062497963450, 84.20452624982236500 ) ) ;
#6608 = ORIENTED_EDGE ( 'NONE', *, *, #3054, .T. ) ;
#6609 = VERTEX_POINT ( 'NONE', #12612 ) ;
#6610 = DIRECTION ( 'NONE',  ( -0.5348440123420857839, -0.8449508165933795611, 0.000000000000000000 ) ) ;
#6611 = DIRECTION ( 'NONE',  ( 1.000000000000000000, 1.156482317317870492E-16, 0.000000000000000000 ) ) ;
#6612 = CIRCLE ( 'NONE', #7595, 0.7892041907098298337 ) ;
#6613 = AXIS2_PLACEMENT_3D ( 'NONE', #8942, #8017, #6704 ) ;
#6614 = CARTESIAN_POINT ( 'NONE',  ( -20.99999999999998579, -2.249290599286302594, -32.99999999999992895 ) ) ;
#6615 = ORIENTED_EDGE ( 'NONE', *, *, #6171, .T. ) ;
#6616 = LINE ( 'NONE', #6473, #932 ) ;
#6617 = CARTESIAN_POINT ( 'NONE',  ( -25.04138923958014473, -6.321889167469157300, 58.00000000000012079 ) ) ;
#6618 = CARTESIAN_POINT ( 'NONE',  ( -2.016677571526633510E-15, 23.25070940071368497, 139.1143251403882459 ) ) ;
#6619 = ORIENTED_EDGE ( 'NONE', *, *, #4321, .F. ) ;
#6620 = DIRECTION ( 'NONE',  ( -0.000000000000000000, 0.000000000000000000, -1.000000000000000000 ) ) ;
#6621 = EDGE_CURVE ( 'NONE', #8767, #14011, #4094, .T. ) ;
#6622 = ADVANCED_FACE ( 'NONE', ( #899 ), #2140, .T. ) ;
#6623 = AXIS2_PLACEMENT_3D ( 'NONE', #400, #9659, #5101 ) ;
#6624 = AXIS2_PLACEMENT_3D ( 'NONE', #14195, #5892, #4645 ) ;
#6625 = CARTESIAN_POINT ( 'NONE',  ( -9.038486528834313916, 1.949452350488303454, 47.50000000626571506 ) ) ;
#6626 = VERTEX_POINT ( 'NONE', #14226 ) ;
#6627 = CARTESIAN_POINT ( 'NONE',  ( -28.95977857253349796, -8.587818791446737876, -48.50000000000012079 ) ) ;
#6628 =( NAMED_UNIT ( * ) SI_UNIT ( $, .STERADIAN. ) SOLID_ANGLE_UNIT ( ) );
#6629 = CARTESIAN_POINT ( 'NONE',  ( 53.54504563787001814, -4.650271872399136086, 48.51982618741349285 ) ) ;
#6630 = CARTESIAN_POINT ( 'NONE',  ( 0.000000000000000000, 21.75070940071312364, -33.00000000000012790 ) ) ;
#6631 = ORIENTED_EDGE ( 'NONE', *, *, #2232, .T. ) ;
#6632 = PLANE ( 'NONE',  #14410 ) ;
#6633 = AXIS2_PLACEMENT_3D ( 'NONE', #1926, #5555, #8014 ) ;
#6634 = FACE_OUTER_BOUND ( 'NONE', #13314, .T. ) ;
#6635 = CARTESIAN_POINT ( 'NONE',  ( 60.45350693790843621, 2.176953084486059176, 60.61639468829817190 ) ) ;
#6636 = CARTESIAN_POINT ( 'NONE',  ( -24.90214939295363550, -6.558472524147630267, -47.52616914649232172 ) ) ;
#6637 = ADVANCED_FACE ( 'NONE', ( #14149 ), #10685, .T. ) ;
#6638 = EDGE_CURVE ( 'NONE', #1585, #11588, #8462, .T. ) ;
#6639 = PRODUCT_RELATED_PRODUCT_CATEGORY ( 'part', '', ( #6577 ) ) ;
#6640 = ORIENTED_EDGE ( 'NONE', *, *, #12153, .F. ) ;
#6641 = CARTESIAN_POINT ( 'NONE',  ( 13.86173033120691223, -69.39711819508849544, 3.619682905202618262 ) ) ;
#6642 = ORIENTED_EDGE ( 'NONE', *, *, #1139, .F. ) ;
#6643 = DIRECTION ( 'NONE',  ( 0.000000000000000000, 1.000000000000000000, 0.000000000000000000 ) ) ;
#6644 = CARTESIAN_POINT ( 'NONE',  ( -65.00000000000001421, -87.24929059928631148, -22.49999999999999289 ) ) ;
#6645 = EDGE_LOOP ( 'NONE', ( #7715, #3936, #4430, #6027 ) ) ;
#6646 = DIRECTION ( 'NONE',  ( 0.8746197071345569451, -0.4848096202550666312, 0.000000000000000000 ) ) ;
#6647 = CYLINDRICAL_SURFACE ( 'NONE', #6543, 3.999999999999999112 ) ;
#6648 = FACE_OUTER_BOUND ( 'NONE', #8315, .T. ) ;
#6649 = VECTOR ( 'NONE', #3066, 1000.000000000000000 ) ;
#6650 = CARTESIAN_POINT ( 'NONE',  ( 11.79472160519158308, -53.28554919726757078, 4.056729053556609621 ) ) ;
#6651 = CARTESIAN_POINT ( 'NONE',  ( 65.71319926014255941, -10.73129157630437547, 77.19766410831374515 ) ) ;
#6652 = DIRECTION ( 'NONE',  ( 0.000000000000000000, -0.000000000000000000, -1.000000000000000000 ) ) ;
#6653 = PLANE ( 'NONE',  #2553 ) ;
#6654 = DIRECTION ( 'NONE',  ( 0.000000000000000000, 0.000000000000000000, -1.000000000000000000 ) ) ;
#6655 = VERTEX_POINT ( 'NONE', #6000 ) ;
#6656 = CARTESIAN_POINT ( 'NONE',  ( 9.950925458496486797, -63.13950256943069661, -2.713503986563631454 ) ) ;
#6657 = VECTOR ( 'NONE', #11799, 1000.000000000000000 ) ;
#6658 = EDGE_LOOP ( 'NONE', ( #15134, #5775, #2998, #11011 ) ) ;
#6659 = CARTESIAN_POINT ( 'NONE',  ( 116.7426776997783406, -40.52765889501078078, 56.28371344025899248 ) ) ;
#6660 = VECTOR ( 'NONE', #13958, 1000.000000000000000 ) ;
#6661 = ORIENTED_EDGE ( 'NONE', *, *, #12289, .T. ) ;
#6662 = CARTESIAN_POINT ( 'NONE',  ( 27.94380378979340662, -67.87804980504306229, 4.252496648647410282 ) ) ;
#6663 = DIRECTION ( 'NONE',  ( -1.000000000000000000, 0.000000000000000000, 0.000000000000000000 ) ) ;
#6664 = DIRECTION ( 'NONE',  ( 1.000000000000000000, -9.251858538542971581E-17, 0.000000000000000000 ) ) ;
#6665 = FACE_OUTER_BOUND ( 'NONE', #3821, .T. ) ;
#6666 = EDGE_CURVE ( 'NONE', #10292, #355, #1366, .T. ) ;
#6667 = CARTESIAN_POINT ( 'NONE',  ( 0.000000000000000000, 0.000000000000000000, -58.00000000000012079 ) ) ;
#6668 = VECTOR ( 'NONE', #9684, 1000.000000000000000 ) ;
#6669 = ORIENTED_EDGE ( 'NONE', *, *, #6298, .F. ) ;
#6670 = VECTOR ( 'NONE', #154, 1000.000000000000000 ) ;
#6671 = EDGE_CURVE ( 'NONE', #10590, #15020, #2528, .T. ) ;
#6672 = CIRCLE ( 'NONE', #1276, 9.999999999999994671 ) ;
#6673 = CARTESIAN_POINT ( 'NONE',  ( 104.0000000000000426, 11.25070940071369563, 139.1143251403882459 ) ) ;
#6674 = CARTESIAN_POINT ( 'NONE',  ( 9.503997712277826082, -53.34604504765411548, -2.388784160331567819 ) ) ;
#6675 = CARTESIAN_POINT ( 'NONE',  ( 130.4454129427046496, 23.25070940071369563, -13.14990448602692474 ) ) ;
#6676 = DIRECTION ( 'NONE',  ( -0.000000000000000000, -0.000000000000000000, -1.000000000000000000 ) ) ;
#6677 = ORIENTED_EDGE ( 'NONE', *, *, #4991, .F. ) ;
#6678 = LINE ( 'NONE', #11217, #14459 ) ;
#6679 = ORIENTED_EDGE ( 'NONE', *, *, #10557, .F. ) ;
#6680 = DIRECTION ( 'NONE',  ( 0.000000000000000000, 0.000000000000000000, 1.000000000000000000 ) ) ;
#6681 = ORIENTED_EDGE ( 'NONE', *, *, #14568, .F. ) ;
#6682 = CIRCLE ( 'NONE', #2012, 2.499999999999995115 ) ;
#6683 = ORIENTED_EDGE ( 'NONE', *, *, #11959, .F. ) ;
#6684 = AXIS2_PLACEMENT_3D ( 'NONE', #5461, #6680, #3147 ) ;
#6685 = EDGE_CURVE ( 'NONE', #4816, #14721, #6149, .T. ) ;
#6686 = VECTOR ( 'NONE', #13388, 1000.000000000000000 ) ;
#6687 = EDGE_CURVE ( 'NONE', #6563, #1582, #11904, .T. ) ;
#6688 = CARTESIAN_POINT ( 'NONE',  ( 9.841896756781917333, -61.30062302791023399, -2.840369378987436022 ) ) ;
#6689 = DIRECTION ( 'NONE',  ( 8.659560562354330119E-17, 0.7071067811865966446, -0.7071067811864982788 ) ) ;
#6690 = VECTOR ( 'NONE', #3611, 1000.000000000000000 ) ;
#6691 = CARTESIAN_POINT ( 'NONE',  ( -5.040221427466109461, 4.089237592873833371, -58.00000000000012079 ) ) ;
#6692 = EDGE_LOOP ( 'NONE', ( #12547, #12948, #6420, #9012, #3778 ) ) ;
#6693 = PLANE ( 'NONE',  #1745 ) ;
#6694 = VECTOR ( 'NONE', #14510, 1000.000000000000000 ) ;
#6695 = CARTESIAN_POINT ( 'NONE',  ( 69.46039030023230509, -2.569771090503329525, 76.19917534039397822 ) ) ;
#6696 = CARTESIAN_POINT ( 'NONE',  ( -9.215065577852303846, 2.268247386559545387, 47.63220435834860922 ) ) ;
#6697 = CARTESIAN_POINT ( 'NONE',  ( 23.78962786808519780, -62.59345883553224610, 6.358786672825899267 ) ) ;
#6698 = EDGE_LOOP ( 'NONE', ( #10226, #8833, #8288, #8365 ) ) ;
#6699 = CARTESIAN_POINT ( 'NONE',  ( 33.62615711857835521, -56.24990207478605697, 2.565511669098800240 ) ) ;
#6700 = AXIS2_PLACEMENT_3D ( 'NONE', #6331, #11024, #8630 ) ;
#6701 = DIRECTION ( 'NONE',  ( -0.000000000000000000, -0.000000000000000000, -1.000000000000000000 ) ) ;
#6702 = ORIENTED_EDGE ( 'NONE', *, *, #7259, .F. ) ;
#6703 = CARTESIAN_POINT ( 'NONE',  ( 104.9938193859979236, 21.75070940071363168, 33.00000000000012790 ) ) ;
#6704 = DIRECTION ( 'NONE',  ( 0.9744556954135514815, -0.2245798247307444206, 0.000000000000000000 ) ) ;
#6705 = DIRECTION ( 'NONE',  ( 0.000000000000000000, 0.000000000000000000, 1.000000000000000000 ) ) ;
#6706 = CYLINDRICAL_SURFACE ( 'NONE', #2269, 31.00000000000000000 ) ;
#6707 = ORIENTED_EDGE ( 'NONE', *, *, #14855, .F. ) ;
#6708 = PRODUCT_DEFINITION_SHAPE ( 'NONE', 'NONE',  #7585 ) ;
#6709 = B_SPLINE_CURVE_WITH_KNOTS ( 'NONE', 3,
 ( #14600, #3762, #593, #9626, #8472, #13157, #1455, #6162, #7382, #12074, #3061, #12604 ),
 .UNSPECIFIED., .F., .F.,
 ( 4, 2, 2, 2, 2, 4 ),
 ( 0.000000000000000000, 0.001071381053236907443, 0.002142762106473816621, 0.003214143159710726016, 0.003749833686329184183, 0.004285524212947642783 ),
 .UNSPECIFIED. ) ;
#6710 = CARTESIAN_POINT ( 'NONE',  ( 52.25109540565180311, -2.012892184189034595, 60.61639468829817190 ) ) ;
#6711 = VECTOR ( 'NONE', #3449, 1000.000000000000000 ) ;
#6712 = EDGE_CURVE ( 'NONE', #4816, #13146, #1444, .T. ) ;
#6713 = CIRCLE ( 'NONE', #97, 4.000000000000000000 ) ;
#6714 = CYLINDRICAL_SURFACE ( 'NONE', #451, 0.5000000000000000000 ) ;
#6715 = CARTESIAN_POINT ( 'NONE',  ( 32.90197589884652274, -57.33450387999030795, 2.749014434309885235 ) ) ;
#6716 = DIRECTION ( 'NONE',  ( 1.000000000000000000, 0.000000000000000000, 0.000000000000000000 ) ) ;
#6717 = PLANE ( 'NONE',  #13796 ) ;
#6718 = EDGE_LOOP ( 'NONE', ( #7372, #14107, #1594, #8452 ) ) ;
#6719 = FACE_OUTER_BOUND ( 'NONE', #6238, .T. ) ;
#6720 = EDGE_LOOP ( 'NONE', ( #243, #14726, #3107, #2212 ) ) ;
#6721 = FACE_OUTER_BOUND ( 'NONE', #12854, .T. ) ;
#6722 = CARTESIAN_POINT ( 'NONE',  ( 95.31453344691183815, 0.000000000000000000, -33.00000000000012790 ) ) ;
#6723 = VECTOR ( 'NONE', #5369, 1000.000000000000000 ) ;
#6724 = ORIENTED_EDGE ( 'NONE', *, *, #10598, .F. ) ;
#6725 = DIRECTION ( 'NONE',  ( 0.000000000000000000, 0.000000000000000000, 1.000000000000000000 ) ) ;
#6726 = CARTESIAN_POINT ( 'NONE',  ( -22.16581936427349575, -2.249290599286303483, 58.00000000000012079 ) ) ;
#6727 = APPLICATION_CONTEXT ( 'automotive_design' ) ;
#6728 = CARTESIAN_POINT ( 'NONE',  ( 100.1541764164548880, 0.000000000000000000, -33.00000000000012790 ) ) ;
#6729 = EDGE_CURVE ( 'NONE', #1441, #6140, #69, .T. ) ;
#6730 = CARTESIAN_POINT ( 'NONE',  ( 30.65234355186507997, 23.25070940071368852, 139.1143251403882459 ) ) ;
#6731 = CARTESIAN_POINT ( 'NONE',  ( 32.46549325755622561, -53.58625433320153064, -2.312436113725388154 ) ) ;
#6732 = CARTESIAN_POINT ( 'NONE',  ( 109.8334623555409735, 0.000000000000000000, 33.00000000000012790 ) ) ;
#6733 = DIRECTION ( 'NONE',  ( 0.000000000000000000, 0.000000000000000000, 1.000000000000000000 ) ) ;
#6734 = CARTESIAN_POINT ( 'NONE',  ( -23.02941217286474185, 4.529839663208023559, -48.26891069786830002 ) ) ;
#6735 = ORIENTED_EDGE ( 'NONE', *, *, #7308, .T. ) ;
#6736 = CARTESIAN_POINT ( 'NONE',  ( -12.33418063572647938, -2.249290599286303927, 50.50000000000012079 ) ) ;
#6737 = ORIENTED_EDGE ( 'NONE', *, *, #11676, .F. ) ;
#6738 = DIRECTION ( 'NONE',  ( 0.000000000000000000, 0.000000000000000000, 1.000000000000000000 ) ) ;
#6739 = ORIENTED_EDGE ( 'NONE', *, *, #2161, .F. ) ;
#6740 = CARTESIAN_POINT ( 'NONE',  ( 13.11526377478540617, -64.14998386711972955, -4.112387283790901904 ) ) ;
#6741 = CARTESIAN_POINT ( 'NONE',  ( 18.24487436548682950, -53.24929059928630437, -6.492462156583989064 ) ) ;
#6742 = EDGE_CURVE ( 'NONE', #6145, #12282, #9784, .T. ) ;
#6743 = FACE_OUTER_BOUND ( 'NONE', #7374, .T. ) ;
#6744 = CYLINDRICAL_SURFACE ( 'NONE', #2056, 2.000000000000000000 ) ;
#6745 = CARTESIAN_POINT ( 'NONE',  ( 88.00000000000002842, 9.769962616701380080E-14, 33.00000000000012790 ) ) ;
#6746 = ORIENTED_EDGE ( 'NONE', *, *, #4021, .T. ) ;
#6747 = FACE_OUTER_BOUND ( 'NONE', #8680, .T. ) ;
#6748 = CARTESIAN_POINT ( 'NONE',  ( 8.397260801138285657, -54.90543917109359029, -2.016464562560237095 ) ) ;
#6749 = CARTESIAN_POINT ( 'NONE',  ( 1.004339113574583608, 0.8906624217387615339, 48.50000000000012079 ) ) ;
#6750 = CARTESIAN_POINT ( 'NONE',  ( 33.25707175001029015, -58.63671304798791084, 1.826958385055428069 ) ) ;
#6751 =( BOUNDED_SURFACE ( )  B_SPLINE_SURFACE ( 3, 2, ( 
 ( #10257, #14951, #2091 ),
 ( #933, #3786, #14108 ),
 ( #8492, #329, #10715 ),
 ( #6107, #14339, #13175 ),
 ( #3851, #9651, #2564 ),
 ( #5957, #9575, #6031 ),
 ( #5023, #2631, #1399 ),
 ( #8556, #10642, #175 ),
 ( #6185, #7021, #107 ),
 ( #7102, #4793, #7325 ) ),
 .UNSPECIFIED., .F., .F., .F. ) 
 B_SPLINE_SURFACE_WITH_KNOTS ( ( 4, 2, 2, 2, 4 ),
 ( 3, 3 ),
 ( 0.0006711510808134562266, 0.001062132081067026709, 0.001453113081320596975, 0.001844094081574167241, 0.002235075081827737724 ),
 ( 0.000000000000000000, 1.000000000000000000 ),
 .UNSPECIFIED. ) 
 GEOMETRIC_REPRESENTATION_ITEM ( )  RATIONAL_B_SPLINE_SURFACE ( (
 ( 1.000000000000000000, 0.7254762501100212591, 1.000000000000000000),
 ( 1.000000000000000000, 0.7255094664176575670, 1.000000000000000000),
 ( 1.000000000000000000, 0.7239949553645330660, 1.000000000000000000),
 ( 1.000000000000000000, 0.7190573720639517052, 1.000000000000000000),
 ( 1.000000000000000000, 0.7156412189950384084, 1.000000000000000000),
 ( 1.000000000000000000, 0.7094102539595253942, 1.000000000000000000),
 ( 1.000000000000000000, 0.7066203625162220670, 1.000000000000000000),
 ( 1.000000000000000000, 0.7042417591948760824, 1.000000000000000000),
 ( 1.000000000000000000, 0.7046402682200600953, 1.000000000000000000),
 ( 1.000000000000000000, 0.7071067811865475727, 1.000000000000000000) ) ) 
 REPRESENTATION_ITEM ( '' )  SURFACE ( )  );
#6752 = VERTEX_POINT ( 'NONE', #12058 ) ;
#6753 = ORIENTED_EDGE ( 'NONE', *, *, #10683, .F. ) ;
#6754 = CARTESIAN_POINT ( 'NONE',  ( 33.38971410812754215, -58.06117559053636512, 1.821720188314281286 ) ) ;
#6755 = ADVANCED_FACE ( 'NONE', ( #13070 ), #9613, .F. ) ;
#6756 = ORIENTED_EDGE ( 'NONE', *, *, #9001, .T. ) ;
#6757 = PLANE ( 'NONE',  #2014 ) ;
#6758 = ORIENTED_EDGE ( 'NONE', *, *, #9567, .T. ) ;
#6759 = LINE ( 'NONE', #5701, #8907 ) ;
#6760 = CARTESIAN_POINT ( 'NONE',  ( 20.86173033120691045, -52.24929059928630437, -3.000000000000000888 ) ) ;
#6761 = SURFACE_STYLE_FILL_AREA ( #4539 ) ;
#6762 = EDGE_CURVE ( 'NONE', #7744, #922, #2371, .T. ) ;
#6763 = ORIENTED_EDGE ( 'NONE', *, *, #5861, .F. ) ;
#6764 = CIRCLE ( 'NONE', #149, 0.7892041907098241715 ) ;
#6765 = FACE_OUTER_BOUND ( 'NONE', #656, .T. ) ;
#6766 = DIRECTION ( 'NONE',  ( 0.000000000000000000, -1.000000000000000000, 0.000000000000000000 ) ) ;
#6767 = CARTESIAN_POINT ( 'NONE',  ( 69.40538204389208943, -3.419623080944494742, 76.98915142890231778 ) ) ;
#6768 = ADVANCED_FACE ( 'NONE', ( #10834 ), #1523, .T. ) ;
#6769 = LINE ( 'NONE', #10239, #1057 ) ;
#6770 = CARTESIAN_POINT ( 'NONE',  ( 23.50212160825726215, -54.09900330344686381, 6.482993899733111576 ) ) ;
#6771 = ADVANCED_FACE ( 'NONE', ( #6228 ), #14075, .F. ) ;
#6772 = VERTEX_POINT ( 'NONE', #14379 ) ;
#6773 = EDGE_CURVE ( 'NONE', #11741, #1508, #3129, .T. ) ;
#6774 = LINE ( 'NONE', #5715, #14186 ) ;
#6775 = LINE ( 'NONE', #10175, #1958 ) ;
#6776 = ORIENTED_EDGE ( 'NONE', *, *, #561, .T. ) ;
#6777 = CARTESIAN_POINT ( 'NONE',  ( 61.93276294469178822, -4.429256696798314685, 87.40005259842790508 ) ) ;
#6778 =( LENGTH_UNIT ( ) NAMED_UNIT ( * ) SI_UNIT ( .MILLI., .METRE. ) );
#6779 = ADVANCED_FACE ( 'NONE', ( #8232 ), #2447, .T. ) ;
#6780 = AXIS2_PLACEMENT_3D ( 'NONE', #7016, #10636, #1240 ) ;
#6781 = CARTESIAN_POINT ( 'NONE',  ( 21.74884261173415467, -85.24929059928631148, 6.000000000000001776 ) ) ;
#6782 = LINE ( 'NONE', #11395, #3017 ) ;
#6783 = ORIENTED_EDGE ( 'NONE', *, *, #8202, .T. ) ;
#6784 = PLANE ( 'NONE',  #2606 ) ;
#6785 = DIRECTION ( 'NONE',  ( -0.000000000000000000, -0.000000000000000000, -1.000000000000000000 ) ) ;
#6786 = CARTESIAN_POINT ( 'NONE',  ( 13.86173033120691223, -69.39711819508849544, 3.619682905202618262 ) ) ;
#6787 = CARTESIAN_POINT ( 'NONE',  ( 58.99998260679605266, 10.75660737539945622, 33.00000000000012790 ) ) ;
#6788 = VECTOR ( 'NONE', #4773, 1000.000000000000000 ) ;
#6789 = FACE_OUTER_BOUND ( 'NONE', #12198, .T. ) ;
#6790 = EDGE_CURVE ( 'NONE', #8699, #13251, #13959, .T. ) ;
#6791 = VECTOR ( 'NONE', #5662, 1000.000000000000000 ) ;
#6792 = VERTEX_POINT ( 'NONE', #9977 ) ;
#6793 = ORIENTED_EDGE ( 'NONE', *, *, #11222, .F. ) ;
#6794 = CARTESIAN_POINT ( 'NONE',  ( 33.03201365928214273, -59.61641240690475740, 2.502824406253571610 ) ) ;
#6795 = AXIS2_PLACEMENT_3D ( 'NONE', #131, #13131, #8446 ) ;
#6796 = EDGE_CURVE ( 'NONE', #4927, #11349, #14209, .T. ) ;
#6797 = ORIENTED_EDGE ( 'NONE', *, *, #7251, .F. ) ;
#6798 = FACE_OUTER_BOUND ( 'NONE', #10210, .T. ) ;
#6799 = CARTESIAN_POINT ( 'NONE',  ( 8.120991012190222236, -55.95216881616708804, 1.883383701763491791 ) ) ;
#6800 = AXIS2_PLACEMENT_3D ( 'NONE', #14181, #5797, #9330 ) ;
#6801 = VERTEX_POINT ( 'NONE', #4115 ) ;
#6802 = CARTESIAN_POINT ( 'NONE',  ( 73.69809405469877106, 29.52935533987996664, 21.00807340887166674 ) ) ;
#6803 = DIRECTION ( 'NONE',  ( 0.6293203910575899673, 0.7771459614506929237, 0.000000000000000000 ) ) ;
#6804 = AXIS2_PLACEMENT_3D ( 'NONE', #4275, #8976, #4127 ) ;
#6805 = CARTESIAN_POINT ( 'NONE',  ( 20.86173033120691045, -52.24929059928630437, 7.000000000000000000 ) ) ;
#6806 = DIRECTION ( 'NONE',  ( -0.000000000000000000, 0.000000000000000000, -1.000000000000000000 ) ) ;
#6807 = CARTESIAN_POINT ( 'NONE',  ( 29.35555050496136431, -52.24929059928631148, -3.199931146564432449 ) ) ;
#6808 = VECTOR ( 'NONE', #3665, 1000.000000000000000 ) ;
#6809 = DIRECTION ( 'NONE',  ( -1.000000000000000000, 0.000000000000000000, 0.000000000000000000 ) ) ;
#6810 = CARTESIAN_POINT ( 'NONE',  ( 52.94134894379979528, -2.395505968190773327, 60.61639468829817190 ) ) ;
#6811 = AXIS2_PLACEMENT_3D ( 'NONE', #12586, #2195, #2038 ) ;
#6812 = FACE_OUTER_BOUND ( 'NONE', #3071, .T. ) ;
#6813 = ORIENTED_EDGE ( 'NONE', *, *, #1123, .T. ) ;
#6814 = FACE_OUTER_BOUND ( 'NONE', #10396, .T. ) ;
#6815 = EDGE_CURVE ( 'NONE', #5948, #14491, #14452, .T. ) ;
#6816 = ADVANCED_FACE ( 'NONE', ( #583 ), #2819, .F. ) ;
#6817 = ORIENTED_EDGE ( 'NONE', *, *, #9886, .T. ) ;
#6818 = DIRECTION ( 'NONE',  ( 1.000000000000000000, 0.000000000000000000, 0.000000000000000000 ) ) ;
#6819 = ORIENTED_EDGE ( 'NONE', *, *, #3873, .T. ) ;
#6820 = DIRECTION ( 'NONE',  ( 1.000000000000000000, 8.673617379884035472E-17, 0.000000000000000000 ) ) ;
#6821 = AXIS2_PLACEMENT_3D ( 'NONE', #7976, #5757, #13977 ) ;
#6822 = CARTESIAN_POINT ( 'NONE',  ( 95.31453344691183815, 23.25070940071369208, -33.00000000000012790 ) ) ;
#6823 = AXIS2_PLACEMENT_3D ( 'NONE', #8211, #5980, #1267 ) ;
#6824 = DIRECTION ( 'NONE',  ( -0.000000000000000000, 0.000000000000000000, -1.000000000000000000 ) ) ;
#6825 = CIRCLE ( 'NONE', #13711, 0.7892041907098288345 ) ;
#6826 = ORIENTED_EDGE ( 'NONE', *, *, #4060, .F. ) ;
#6827 = FACE_OUTER_BOUND ( 'NONE', #5361, .T. ) ;
#6828 = CARTESIAN_POINT ( 'NONE',  ( 9.357522953353912598, -54.69330887924044049, -3.128542914574955702 ) ) ;
#6829 = DIRECTION ( 'NONE',  ( -0.000000000000000000, -0.000000000000000000, -1.000000000000000000 ) ) ;
#6830 = CARTESIAN_POINT ( 'NONE',  ( -10.96079405803985729, -9.021238043844263643, 48.26696389624903816 ) ) ;
#6831 = ORIENTED_EDGE ( 'NONE', *, *, #3303, .F. ) ;
#6832 = ADVANCED_FACE ( 'NONE', ( #1815 ), #13586, .T. ) ;
#6833 = ADVANCED_FACE ( 'NONE', ( #1880 ), #12202, .F. ) ;
#6834 = DIRECTION ( 'NONE',  ( -0.000000000000000000, 0.000000000000000000, 1.000000000000000000 ) ) ;
#6835 = PRODUCT_RELATED_PRODUCT_CATEGORY ( 'part', '', ( #2889 ) ) ;
#6836 = ORIENTED_EDGE ( 'NONE', *, *, #13014, .T. ) ;
#6837 = LINE ( 'NONE', #8991, #1284 ) ;
#6838 = AXIS2_PLACEMENT_3D ( 'NONE', #4225, #9946, #6537 ) ;
#6839 = VERTEX_POINT ( 'NONE', #5357 ) ;
#6840 = DIRECTION ( 'NONE',  ( 0.000000000000000000, -1.445602896647339163E-16, 1.000000000000000000 ) ) ;
#6841 = CARTESIAN_POINT ( 'NONE',  ( -24.72817752516935741, 2.363221963240438761, -48.00000000000019185 ) ) ;
#6842 = CARTESIAN_POINT ( 'NONE',  ( 10.85795585539533370, -53.50274931745887841, -3.718097397461419540 ) ) ;
#6843 = VERTEX_POINT ( 'NONE', #7667 ) ;
#6844 = DIRECTION ( 'NONE',  ( 1.000000000000000000, 0.000000000000000000, 0.000000000000000000 ) ) ;
#6845 = CARTESIAN_POINT ( 'NONE',  ( 58.00000000000000711, -2.249290599286311032, 36.00000000000012079 ) ) ;
#6846 = CARTESIAN_POINT ( 'NONE',  ( 76.00751999314820750, -6.514251586541772276, 71.19766410831374515 ) ) ;
#6847 = VECTOR ( 'NONE', #2233, 1000.000000000000000 ) ;
#6848 = CARTESIAN_POINT ( 'NONE',  ( 29.69047892279255763, -53.28399145779480506, 4.141535524925023637 ) ) ;
#6849 = CARTESIAN_POINT ( 'NONE',  ( 23.93808696748067177, -66.03679020170480385, 6.288305159851943493 ) ) ;
#6850 = ORIENTED_EDGE ( 'NONE', *, *, #4629, .F. ) ;
#6851 = DIRECTION ( 'NONE',  ( -1.000000000000000000, 0.000000000000000000, 0.000000000000000000 ) ) ;
#6852 = PLANE ( 'NONE',  #8120 ) ;
#6853 = EDGE_CURVE ( 'NONE', #5462, #8536, #6433, .T. ) ;
#6854 = ORIENTED_EDGE ( 'NONE', *, *, #684, .F. ) ;
#6855 = DIRECTION ( 'NONE',  ( 1.000000000000000000, 0.000000000000000000, 0.000000000000000000 ) ) ;
#6856 = CIRCLE ( 'NONE', #5900, 4.165819364273509962 ) ;
#6857 = FILL_AREA_STYLE ('',( #10412 ) ) ;
#6858 = AXIS2_PLACEMENT_3D ( 'NONE', #6635, #11250, #702 ) ;
#6859 = VERTEX_POINT ( 'NONE', #3898 ) ;
#6860 = CARTESIAN_POINT ( 'NONE',  ( -9.037775043065352065, 2.932694901963889489, 57.50000000000012079 ) ) ;
#6861 = DIRECTION ( 'NONE',  ( 0.000000000000000000, 1.000000000000000000, -0.000000000000000000 ) ) ;
#6862 = ORIENTED_EDGE ( 'NONE', *, *, #5039, .T. ) ;
#6863 = PLANE ( 'NONE',  #14157 ) ;
#6864 = CARTESIAN_POINT ( 'NONE',  ( 0.000000000000000000, 0.000000000000000000, -33.00000000000012790 ) ) ;
#6865 = LINE ( 'NONE', #782, #2659 ) ;
#6866 = CARTESIAN_POINT ( 'NONE',  ( 100.0000000000000284, 11.25070940071369563, 33.00000000000012790 ) ) ;
#6867 = FACE_OUTER_BOUND ( 'NONE', #915, .T. ) ;
#6868 = EDGE_CURVE ( 'NONE', #13646, #7307, #14736, .T. ) ;
#6869 = VECTOR ( 'NONE', #6197, 1000.000000000000000 ) ;
#6870 = DIRECTION ( 'NONE',  ( 0.000000000000000000, 0.000000000000000000, 1.000000000000000000 ) ) ;
#6871 = ORIENTED_EDGE ( 'NONE', *, *, #12821, .T. ) ;
#6872 = B_SPLINE_CURVE_WITH_KNOTS ( 'NONE', 3,
 ( #7570, #8869, #3035, #9889, #14573, #5186, #8715, #12264, #7727, #1861 ),
 .UNSPECIFIED., .F., .F.,
 ( 4, 2, 2, 2, 4 ),
 ( 0.000000000000000000, 0.002335515930058447605, 0.004671031860116895210, 0.007006547790175342814, 0.009342063720233790419 ),
 .UNSPECIFIED. ) ;
#6873 = ORIENTED_EDGE ( 'NONE', *, *, #3343, .T. ) ;
#6874 = AXIS2_PLACEMENT_3D ( 'NONE', #7250, #12014, #13177 ) ;
#6875 = CARTESIAN_POINT ( 'NONE',  ( 32.18398686573303991, -61.03341231845916326, 2.731818205568650626 ) ) ;
#6876 = ORIENTED_EDGE ( 'NONE', *, *, #11805, .T. ) ;
#6877 = CARTESIAN_POINT ( 'NONE',  ( 9.566432878864672418, -53.28273180918434804, -2.408293854232251174 ) ) ;
#6878 = CARTESIAN_POINT ( 'NONE',  ( 62.67308791069655882, 29.52935533987996664, -33.00000000000013500 ) ) ;
#6879 = ORIENTED_EDGE ( 'NONE', *, *, #1296, .T. ) ;
#6880 = CARTESIAN_POINT ( 'NONE',  ( 67.21328690825531282, 25.52935533987996664, 84.20452624982236500 ) ) ;
#6881 = LINE ( 'NONE', #2191, #4087 ) ;
#6882 = EDGE_CURVE ( 'NONE', #1679, #13146, #4187, .T. ) ;
#6883 = CIRCLE ( 'NONE', #260, 11.46463184759104870 ) ;
#6884 = EDGE_CURVE ( 'NONE', #1311, #12875, #671, .T. ) ;
#6885 = CARTESIAN_POINT ( 'NONE',  ( 80.00000000000001421, -85.24929059928631148, 6.000000000000001776 ) ) ;
#6886 = CARTESIAN_POINT ( 'NONE',  ( -16.99999999999998579, -2.249290599286303927, 47.50000000000012079 ) ) ;
#6887 = DIRECTION ( 'NONE',  ( 1.000000000000000000, 0.000000000000000000, 0.000000000000000000 ) ) ;
#6888 = DIRECTION ( 'NONE',  ( -1.156482317317870492E-16, 1.000000000000000000, -0.000000000000000000 ) ) ;
#6889 = CARTESIAN_POINT ( 'NONE',  ( 10.23047706855496841, -60.71197230342421136, 3.050751728647412175 ) ) ;
#6890 = CARTESIAN_POINT ( 'NONE',  ( 12.36791015745246192, -53.24929059928630437, 3.199931146564420903 ) ) ;
#6891 = ORIENTED_EDGE ( 'NONE', *, *, #8572, .T. ) ;
#6892 = CARTESIAN_POINT ( 'NONE',  ( 13.25069131558226232, -58.78589452312201047, -4.200179654064304380 ) ) ;
#6893 = UNCERTAINTY_MEASURE_WITH_UNIT (LENGTH_MEASURE( 1.000000000000000082E-05 ), #1493, 'distance_accuracy_value', 'NONE');
#6894 = VERTEX_POINT ( 'NONE', #8731 ) ;
#6895 = CARTESIAN_POINT ( 'NONE',  ( 8.091875466796944139, -56.52532528994245808, 1.842181053809107238 ) ) ;
#6896 = VERTEX_POINT ( 'NONE', #10051 ) ;
#6897 = FILL_AREA_STYLE ('',( #13824 ) ) ;
#6898 = CARTESIAN_POINT ( 'NONE',  ( 27.84961282986260400, -69.39711819508849544, 3.799217554615836878 ) ) ;
#6899 = DIRECTION ( 'NONE',  ( 0.000000000000000000, 0.000000000000000000, -1.000000000000000000 ) ) ;
#6900 = AXIS2_PLACEMENT_3D ( 'NONE', #9675, #14363, #13200 ) ;
#6901 = CARTESIAN_POINT ( 'NONE',  ( 18.24487436548683306, -52.24929059928629727, -6.492462156583990840 ) ) ;
#6902 = B_SPLINE_CURVE_WITH_KNOTS ( 'NONE', 3,
 ( #12885, #4941, #11634, #9486, #173, #11709, #7173, #4865, #9650, #3557 ),
 .UNSPECIFIED., .F., .F.,
 ( 4, 2, 2, 2, 4 ),
 ( 8.673617379884034509E-19, 0.002320432257317494879, 0.004640864514634988891, 0.006961296771952482469, 0.009281729029269976047 ),
 .UNSPECIFIED. ) ;
#6903 = ORIENTED_EDGE ( 'NONE', *, *, #15074, .T. ) ;
#6904 = EDGE_CURVE ( 'NONE', #3904, #4172, #12138, .T. ) ;
#6905 = DIRECTION ( 'NONE',  ( 1.000000000000000000, 0.000000000000000000, 0.000000000000000000 ) ) ;
#6906 = CARTESIAN_POINT ( 'NONE',  ( 9.222151644637104795, -54.90141807276702224, -3.067753764789347581 ) ) ;
#6907 = CARTESIAN_POINT ( 'NONE',  ( 48.84742675818896629, 2.824063592853376381, 82.40005259842790508 ) ) ;
#6908 = EDGE_CURVE ( 'NONE', #3756, #9345, #14659, .T. ) ;
#6909 = DIRECTION ( 'NONE',  ( -0.8208219420614786266, 0.4549890321264269399, 0.3453061251629919171 ) ) ;
#6910 = VERTEX_POINT ( 'NONE', #8592 ) ;
#6911 = AXIS2_PLACEMENT_3D ( 'NONE', #12961, #10494, #15190 ) ;
#6912 = VERTEX_POINT ( 'NONE', #6362 ) ;
#6913 = CIRCLE ( 'NONE', #13542, 0.5000000000000004441 ) ;
#6914 = DIRECTION ( 'NONE',  ( 1.000000000000000000, 0.000000000000000000, 0.000000000000000000 ) ) ;
#6915 = ORIENTED_EDGE ( 'NONE', *, *, #11959, .T. ) ;
#6916 = LINE ( 'NONE', #13688, #12077 ) ;
#6917 = ORIENTED_EDGE ( 'NONE', *, *, #9956, .T. ) ;
#6918 = ORIENTED_EDGE ( 'NONE', *, *, #9835, .F. ) ;
#6919 = VECTOR ( 'NONE', #10442, 1000.000000000000000 ) ;
#6920 = CARTESIAN_POINT ( 'NONE',  ( -22.94555154978778688, 4.515786682032536525, -48.04486892757390848 ) ) ;
#6921 = VERTEX_POINT ( 'NONE', #7514 ) ;
#6922 = VECTOR ( 'NONE', #12220, 1000.000000000000000 ) ;
#6923 = VECTOR ( 'NONE', #10962, 1000.000000000000000 ) ;
#6924 = CARTESIAN_POINT ( 'NONE',  ( -8.537170960192302260, 2.067018546614596719, 47.50000000000012079 ) ) ;
#6925 = LINE ( 'NONE', #9884, #4467 ) ;
#6926 = EDGE_CURVE ( 'NONE', #8444, #13835, #1891, .T. ) ;
#6927 = ORIENTED_EDGE ( 'NONE', *, *, #9809, .F. ) ;
#6928 = EDGE_CURVE ( 'NONE', #8234, #8468, #11126, .T. ) ;
#6929 = DIRECTION ( 'NONE',  ( -0.000000000000000000, -0.000000000000000000, -1.000000000000000000 ) ) ;
#6930 = CARTESIAN_POINT ( 'NONE',  ( 64.11356537427461433, -11.94785244191377949, 72.92170383108769727 ) ) ;
#6931 = PLANE ( 'NONE',  #6475 ) ;
#6932 = CARTESIAN_POINT ( 'NONE',  ( 34.22640527878306216, -51.17811635680435955, 2.733205671951302040 ) ) ;
#6933 = EDGE_LOOP ( 'NONE', ( #1218, #3843, #14227, #2048 ) ) ;
#6934 = MECHANICAL_DESIGN_GEOMETRIC_PRESENTATION_REPRESENTATION (  '', ( #12580 ), #12335 ) ;
#6935 = DIRECTION ( 'NONE',  ( -0.000000000000000000, -0.000000000000000000, -1.000000000000000000 ) ) ;
#6936 = VECTOR ( 'NONE', #10460, 1000.000000000000000 ) ;
#6937 = CIRCLE ( 'NONE', #781, 4.665819364273509073 ) ;
#6938 = ORIENTED_EDGE ( 'NONE', *, *, #6882, .F. ) ;
#6939 = DIRECTION ( 'NONE',  ( -0.8746197071345569451, 0.4848096202550666312, 0.000000000000000000 ) ) ;
#6940 = DIRECTION ( 'NONE',  ( -0.000000000000000000, 0.000000000000000000, 1.000000000000000000 ) ) ;
#6941 = ORIENTED_EDGE ( 'NONE', *, *, #12136, .F. ) ;
#6942 = DIRECTION ( 'NONE',  ( 1.000000000000000000, 0.000000000000000000, 0.000000000000000000 ) ) ;
#6943 = FACE_OUTER_BOUND ( 'NONE', #13609, .T. ) ;
#6944 = CARTESIAN_POINT ( 'NONE',  ( 93.56770215592470663, 23.25070940071369208, -33.00000000000012790 ) ) ;
#6945 = ORIENTED_EDGE ( 'NONE', *, *, #12274, .T. ) ;
#6946 = EDGE_CURVE ( 'NONE', #14830, #5864, #10982, .T. ) ;
#6947 = CARTESIAN_POINT ( 'NONE',  ( 40.00000000000001421, 23.95881716715930665, -32.99999999999982947 ) ) ;
#6948 = CIRCLE ( 'NONE', #11353, 0.5000000000000004441 ) ;
#6949 = CARTESIAN_POINT ( 'NONE',  ( 64.90552635791956959, 22.43695620243006772, -33.00000000000012790 ) ) ;
#6950 = VECTOR ( 'NONE', #4452, 1000.000000000000000 ) ;
#6951 = CARTESIAN_POINT ( 'NONE',  ( 9.233977672013530480, -60.63235088943247320, 1.938839523630885298 ) ) ;
#6952 = CARTESIAN_POINT ( 'NONE',  ( -8.842479278987921631, -7.118053859731281463, -48.00000000000012079 ) ) ;
#6953 = VECTOR ( 'NONE', #13330, 1000.000000000000000 ) ;
#6954 = DIRECTION ( 'NONE',  ( 0.000000000000000000, 0.000000000000000000, -1.000000000000000000 ) ) ;
#6955 = DIRECTION ( 'NONE',  ( 0.000000000000000000, 0.000000000000000000, 1.000000000000000000 ) ) ;
#6956 = ORIENTED_EDGE ( 'NONE', *, *, #8609, .T. ) ;
#6957 = ORIENTED_EDGE ( 'NONE', *, *, #10179, .T. ) ;
#6958 = CARTESIAN_POINT ( 'NONE',  ( 31.72322230991231962, -61.42570632716525125, 2.132522520905399954 ) ) ;
#6959 = ORIENTED_EDGE ( 'NONE', *, *, #4471, .T. ) ;
#6960 = CARTESIAN_POINT ( 'NONE',  ( 31.10334365618822261, -60.64100864355886955, 2.132522520905398622 ) ) ;
#6961 = DIRECTION ( 'NONE',  ( 0.000000000000000000, 0.000000000000000000, 1.000000000000000000 ) ) ;
#6962 = ORIENTED_EDGE ( 'NONE', *, *, #1365, .T. ) ;
#6963 = DIRECTION ( 'NONE',  ( 0.5006040828730989878, -0.8656763553492631269, 0.000000000000000000 ) ) ;
#6964 = CARTESIAN_POINT ( 'NONE',  ( 20.86173033120691045, -96.56299909827106376, 0.000000000000000000 ) ) ;
#6965 = CIRCLE ( 'NONE', #10405, 3.999999999999999112 ) ;
#6966 = EDGE_CURVE ( 'NONE', #5141, #4878, #8782, .T. ) ;
#6967 = SURFACE_SIDE_STYLE ('',( #5978 ) ) ;
#6968 = FACE_OUTER_BOUND ( 'NONE', #13690, .T. ) ;
#6969 = CARTESIAN_POINT ( 'NONE',  ( -16.99999999999998579, -2.249290599286303927, -47.50000000000012079 ) ) ;
#6970 = DIRECTION ( 'NONE',  ( 0.000000000000000000, 1.682156097916903736E-15, -1.000000000000000000 ) ) ;
#6971 = CARTESIAN_POINT ( 'NONE',  ( 9.200644618036294631, -59.06479067038043240, 2.757123406423048984 ) ) ;
#6972 = CYLINDRICAL_SURFACE ( 'NONE', #4109, 0.7892041907098262810 ) ;
#6973 = AXIS2_PLACEMENT_3D ( 'NONE', #8069, #6909, #5689 ) ;
#6974 = EDGE_CURVE ( 'NONE', #8990, #10346, #5741, .T. ) ;
#6975 = ORIENTED_EDGE ( 'NONE', *, *, #11701, .T. ) ;
#6976 = EDGE_CURVE ( 'NONE', #4729, #10905, #15131, .T. ) ;
#6977 = CARTESIAN_POINT ( 'NONE',  ( 65.00000000000001421, -85.24929059928629727, -19.99999999999999645 ) ) ;
#6978 = ORIENTED_EDGE ( 'NONE', *, *, #10774, .F. ) ;
#6979 = CARTESIAN_POINT ( 'NONE',  ( 100.0000000000000284, 6.750709400713692965, 33.00000000000012790 ) ) ;
#6980 = ORIENTED_EDGE ( 'NONE', *, *, #622, .T. ) ;
#6981 = DIRECTION ( 'NONE',  ( -1.000000000000000000, -8.673617379884035472E-17, 0.000000000000000000 ) ) ;
#6982 = EDGE_LOOP ( 'NONE', ( #9380, #11074, #4292, #11931 ) ) ;
#6983 = CARTESIAN_POINT ( 'NONE',  ( 64.69561927709757754, -11.57345611214739733, 75.63685169989432211 ) ) ;
#6984 = DIRECTION ( 'NONE',  ( -0.000000000000000000, -0.000000000000000000, -1.000000000000000000 ) ) ;
#6985 = ADVANCED_FACE ( 'NONE', ( #11345 ), #15056, .F. ) ;
#6986 = CARTESIAN_POINT ( 'NONE',  ( 23.63986771004770304, -58.63441909321034728, -6.426091441073434218 ) ) ;
#6987 = ORIENTED_EDGE ( 'NONE', *, *, #4000, .T. ) ;
#6988 = CARTESIAN_POINT ( 'NONE',  ( 8.199792978590132009, -57.47994873761392398, -2.501453769636593716 ) ) ;
#6989 = CARTESIAN_POINT ( 'NONE',  ( 10.26865515301073728, -52.78690463905002872, -2.615816816691508784 ) ) ;
#6990 = PLANE ( 'NONE',  #13584 ) ;
#6991 = CARTESIAN_POINT ( 'NONE',  ( -12.14523415828296216, -9.827631355817223024, 48.00000000000012079 ) ) ;
#6992 = ORIENTED_EDGE ( 'NONE', *, *, #14702, .T. ) ;
#6993 = ORIENTED_EDGE ( 'NONE', *, *, #5626, .F. ) ;
#6994 = CARTESIAN_POINT ( 'NONE',  ( 118.5627027169299765, -35.81974489651393156, 54.40673322733726280 ) ) ;
#6995 = VERTEX_POINT ( 'NONE', #13662 ) ;
#6996 = DIRECTION ( 'NONE',  ( -0.8420378618367728718, -0.5394184268574404584, -0.000000000000000000 ) ) ;
#6997 = ORIENTED_EDGE ( 'NONE', *, *, #8732, .T. ) ;
#6998 = EDGE_CURVE ( 'NONE', #6293, #11451, #1170, .T. ) ;
#6999 = ORIENTED_EDGE ( 'NONE', *, *, #6309, .F. ) ;
#7000 = DIRECTION ( 'NONE',  ( -0.000000000000000000, -1.000000000000000000, -1.734723475976817547E-15 ) ) ;
#7001 = CYLINDRICAL_SURFACE ( 'NONE', #3256, 0.7892041907098262810 ) ;
#7002 = ORIENTED_EDGE ( 'NONE', *, *, #2638, .F. ) ;
#7003 = DIRECTION ( 'NONE',  ( -0.8656763553492639041, -0.5006040828730973224, 0.000000000000000000 ) ) ;
#7004 = CARTESIAN_POINT ( 'NONE',  ( 76.30953153521004140, -6.681659317953794641, 72.13615421477459222 ) ) ;
#7005 = EDGE_LOOP ( 'NONE', ( #7278, #13914, #3121, #1042 ) ) ;
#7006 = CARTESIAN_POINT ( 'NONE',  ( -80.00000000000001421, -85.24929059928629727, -32.00000000000000000 ) ) ;
#7007 = FACE_OUTER_BOUND ( 'NONE', #4325, .T. ) ;
#7008 = CARTESIAN_POINT ( 'NONE',  ( 45.17127246049422240, 23.25070940071368852, 33.00000000000012790 ) ) ;
#7009 = CARTESIAN_POINT ( 'NONE',  ( 28.99759814586801454, -51.89519585609026109, 4.215672595248425303 ) ) ;
#7010 = ORIENTED_EDGE ( 'NONE', *, *, #570, .F. ) ;
#7011 = CARTESIAN_POINT ( 'NONE',  ( 50.01091543003727224, 21.75070940071325865, 139.1143251403882459 ) ) ;
#7012 = EDGE_CURVE ( 'NONE', #3688, #4595, #9417, .T. ) ;
#7013 = ORIENTED_EDGE ( 'NONE', *, *, #7991, .F. ) ;
#7014 = ADVANCED_FACE ( 'NONE', ( #3432 ), #6972, .T. ) ;
#7015 = CARTESIAN_POINT ( 'NONE',  ( 118.0000000000000568, 2.046973701652633381E-13, 33.00000000000012790 ) ) ;
#7016 = CARTESIAN_POINT ( 'NONE',  ( 59.59091026602544616, -7.053490217115945704, 60.61639468829817190 ) ) ;
#7017 = DIRECTION ( 'NONE',  ( 1.000000000000000000, 0.000000000000000000, 0.000000000000000000 ) ) ;
#7018 = CARTESIAN_POINT ( 'NONE',  ( 8.332112475569905641, -58.05408529505802306, 2.501672671478884169 ) ) ;
#7019 = PLANE ( 'NONE',  #2015 ) ;
#7020 = VERTEX_POINT ( 'NONE', #3350 ) ;
#7021 = CARTESIAN_POINT ( 'NONE',  ( -9.009135308666337494, 1.891904487837172688, -48.00342231809197102 ) ) ;
#7022 = CARTESIAN_POINT ( 'NONE',  ( 33.03128477131276952, -59.61959967696117246, -2.502829331418514602 ) ) ;
#7023 = DIRECTION ( 'NONE',  ( 1.000000000000000000, 0.000000000000000000, 0.000000000000000000 ) ) ;
#7024 = CARTESIAN_POINT ( 'NONE',  ( 80.00000000000001421, -74.24929059928631148, -32.00000000000000000 ) ) ;
#7025 = DIRECTION ( 'NONE',  ( -0.000000000000000000, 0.000000000000000000, -1.000000000000000000 ) ) ;
#7026 = LINE ( 'NONE', #4564, #14299 ) ;
#7027 = ORIENTED_EDGE ( 'NONE', *, *, #12056, .F. ) ;
#7028 = ORIENTED_EDGE ( 'NONE', *, *, #335, .T. ) ;
#7029 = EDGE_CURVE ( 'NONE', #15091, #7237, #5108, .T. ) ;
#7030 = VECTOR ( 'NONE', #7565, 1000.000000000000000 ) ;
#7031 = CARTESIAN_POINT ( 'NONE',  ( 104.9938193859979236, 23.25070940071369208, 139.1143251403882459 ) ) ;
#7032 = EDGE_CURVE ( 'NONE', #1828, #6079, #6105, .T. ) ;
#7033 = VERTEX_POINT ( 'NONE', #10437 ) ;
#7034 = PLANE ( 'NONE',  #7658 ) ;
#7035 = CARTESIAN_POINT ( 'NONE',  ( 42.07846078193830408, 0.000000000000000000, 139.1143251403882459 ) ) ;
#7036 = FACE_OUTER_BOUND ( 'NONE', #7219, .T. ) ;
#7037 = DIRECTION ( 'NONE',  ( 0.8656763553493069807, 0.5006040828730229375, -0.000000000000000000 ) ) ;
#7038 = DIRECTION ( 'NONE',  ( 0.000000000000000000, 0.000000000000000000, 1.000000000000000000 ) ) ;
#7039=STYLED_ITEM('',(#15258),#9491);
#7040 = CARTESIAN_POINT ( 'NONE',  ( 32.39917484285220439, 23.25070940071368852, 139.1143251403882459 ) ) ;
#7041 = CARTESIAN_POINT ( 'NONE',  ( -24.64572710697934710, -6.998028550906933098, 47.88483805351501132 ) ) ;
#7042 = CARTESIAN_POINT ( 'NONE',  ( 9.411927710346049025, -59.69665779701217190, 2.790274538705358687 ) ) ;
#7043 = CARTESIAN_POINT ( 'NONE',  ( 33.18918945647200758, -54.61739641898385145, 2.842377187920258397 ) ) ;
#7044 = VERTEX_POINT ( 'NONE', #8968 ) ;
#7045 = B_SPLINE_CURVE_WITH_KNOTS ( 'NONE', 3,
 ( #14714, #1713, #13340, #14567 ),
 .UNSPECIFIED., .F., .F.,
 ( 4, 4 ),
 ( 0.000000000000000000, 0.001771943201165730340 ),
 .UNSPECIFIED. ) ;
#7046 = DIRECTION ( 'NONE',  ( 0.000000000000000000, 0.000000000000000000, 1.000000000000000000 ) ) ;
#7047 = PRODUCT_DEFINITION_CONTEXT ( 'detailed design', #6727, 'design' ) ;
#7048 = ORIENTED_EDGE ( 'NONE', *, *, #7721, .T. ) ;
#7049 = CARTESIAN_POINT ( 'NONE',  ( 32.52281604437752804, -59.06479067038043240, 2.757123406423070744 ) ) ;
#7050 = VECTOR ( 'NONE', #13081, 1000.000000000000000 ) ;
#7051 = ORIENTED_EDGE ( 'NONE', *, *, #14956, .T. ) ;
#7052 = AXIS2_PLACEMENT_3D ( 'NONE', #4901, #14219, #12993 ) ;
#7053 = ORIENTED_EDGE ( 'NONE', *, *, #196, .F. ) ;
#7054 = DIRECTION ( 'NONE',  ( 0.000000000000000000, 0.000000000000000000, -1.000000000000000000 ) ) ;
#7055 = EDGE_CURVE ( 'NONE', #14936, #4250, #10357, .T. ) ;
#7056 = FACE_OUTER_BOUND ( 'NONE', #832, .T. ) ;
#7057 = LINE ( 'NONE', #1281, #2770 ) ;
#7058 = VECTOR ( 'NONE', #11894, 1000.000000000000000 ) ;
#7059 = EDGE_CURVE ( 'NONE', #7490, #170, #14683, .T. ) ;
#7060 = VECTOR ( 'NONE', #3422, 1000.000000000000000 ) ;
#7061 = EDGE_CURVE ( 'NONE', #6839, #5660, #5518, .T. ) ;
#7062 = ORIENTED_EDGE ( 'NONE', *, *, #10491, .T. ) ;
#7063 = AXIS2_PLACEMENT_3D ( 'NONE', #10433, #5666, #9206 ) ;
#7064 = TOROIDAL_SURFACE ( 'NONE', #426, 9.500000000000001776, 0.5000000000000000000 ) ;
#7065 = DIRECTION ( 'NONE',  ( 0.000000000000000000, 0.000000000000000000, 1.000000000000000000 ) ) ;
#7066 = DIRECTION ( 'NONE',  ( -0.000000000000000000, -0.000000000000000000, 1.000000000000000000 ) ) ;
#7067 = DIRECTION ( 'NONE',  ( 1.000000000000000000, 0.000000000000000000, 0.000000000000000000 ) ) ;
#7068 = EDGE_CURVE ( 'NONE', #12778, #844, #4345, .T. ) ;
#7069 = ORIENTED_EDGE ( 'NONE', *, *, #11053, .T. ) ;
#7070 = EDGE_CURVE ( 'NONE', #8978, #2280, #7324, .T. ) ;
#7071 = ORIENTED_EDGE ( 'NONE', *, *, #5945, .F. ) ;
#7072 = CARTESIAN_POINT ( 'NONE',  ( -3.190546569013415379, 0.8906624217387615339, -48.00000000000012079 ) ) ;
#7073 = ORIENTED_EDGE ( 'NONE', *, *, #11338, .F. ) ;
#7074 = PLANE ( 'NONE',  #4705 ) ;
#7075 = VECTOR ( 'NONE', #1670, 1000.000000000000000 ) ;
#7076 = CARTESIAN_POINT ( 'NONE',  ( 14.02634622330045744, -66.46764508687286366, 4.441229594909811063 ) ) ;
#7077 = ORIENTED_EDGE ( 'NONE', *, *, #8626, .F. ) ;
#7078 = AXIS2_PLACEMENT_3D ( 'NONE', #5787, #9243, #6844 ) ;
#7079 = ORIENTED_EDGE ( 'NONE', *, *, #10546, .T. ) ;
#7080 = VECTOR ( 'NONE', #9102, 1000.000000000000000 ) ;
#7081 = DIRECTION ( 'NONE',  ( 1.000000000000000000, 0.000000000000000000, 0.000000000000000000 ) ) ;
#7082 = DIRECTION ( 'NONE',  ( 1.000000000000000000, 0.000000000000000000, 0.000000000000000000 ) ) ;
#7083 = EDGE_CURVE ( 'NONE', #4346, #1838, #3196, .T. ) ;
#7084 = ADVANCED_FACE ( 'NONE', ( #6812 ), #2645, .T. ) ;
#7085 = CARTESIAN_POINT ( 'NONE',  ( 23.10474973039556801, -52.24929059928630437, -5.564967562786268473 ) ) ;
#7086 = CARTESIAN_POINT ( 'NONE',  ( -8.754378065084850391, 2.456381933588792865, 48.23869654929341522 ) ) ;
#7087 = ORIENTED_EDGE ( 'NONE', *, *, #14806, .F. ) ;
#7088 = AXIS2_PLACEMENT_3D ( 'NONE', #4212, #3992, #13456 ) ;
#7089 = CARTESIAN_POINT ( 'NONE',  ( 20.86173033120691045, -53.24929059928630437, 0.000000000000000000 ) ) ;
#7090 = LINE ( 'NONE', #161, #9383 ) ;
#7091 = CARTESIAN_POINT ( 'NONE',  ( -65.00000000000001421, -85.24929059928629727, -19.99999999999999645 ) ) ;
#7092 = AXIS2_PLACEMENT_3D ( 'NONE', #2332, #12806, #5734 ) ;
#7093 = VERTEX_POINT ( 'NONE', #9130 ) ;
#7094 = CARTESIAN_POINT ( 'NONE',  ( 69.32915027133518038, -4.025971040916268784, 72.13752247958439057 ) ) ;
#7095 = ORIENTED_EDGE ( 'NONE', *, *, #5180, .F. ) ;
#7096 = LINE ( 'NONE', #99, #1027 ) ;
#7097 =( LENGTH_UNIT ( ) NAMED_UNIT ( * ) SI_UNIT ( .MILLI., .METRE. ) );
#7098 = ORIENTED_EDGE ( 'NONE', *, *, #10420, .F. ) ;
#7099 = CARTESIAN_POINT ( 'NONE',  ( -24.72817752516938228, 2.363221963240404566, -47.50000000000012079 ) ) ;
#7100 = DIRECTION ( 'NONE',  ( -0.000000000000000000, 0.000000000000000000, -1.000000000000000000 ) ) ;
#7101 = ORIENTED_EDGE ( 'NONE', *, *, #2016, .F. ) ;
#7102 = CARTESIAN_POINT ( 'NONE',  ( -8.537170960192302260, 2.067018546614597163, -48.00000000000012079 ) ) ;
#7103 = DIRECTION ( 'NONE',  ( -1.000000000000000000, 0.000000000000000000, 0.000000000000000000 ) ) ;
#7104 = DIRECTION ( 'NONE',  ( -0.8746197071345569451, 0.4848096202550666312, 0.000000000000000000 ) ) ;
#7105 = CARTESIAN_POINT ( 'NONE',  ( 28.24717992610507622, -64.89641169172455193, 4.245552436241676553 ) ) ;
#7106 = EDGE_CURVE ( 'NONE', #9234, #8992, #10287, .T. ) ;
#7107 = CARTESIAN_POINT ( 'NONE',  ( 9.200644618036294631, -59.06479067038043240, 2.757123406423048984 ) ) ;
#7108 = CARTESIAN_POINT ( 'NONE',  ( 31.49680259653621306, -53.84195147944124216, -3.481029309662088789 ) ) ;
#7109 = VERTEX_POINT ( 'NONE', #5825 ) ;
#7110 = CARTESIAN_POINT ( 'NONE',  ( 58.00000000000000711, -2.249290599286309256, 77.19766410831374515 ) ) ;
#7111 = ORIENTED_EDGE ( 'NONE', *, *, #6712, .T. ) ;
#7112 = DIRECTION ( 'NONE',  ( -0.6198786537240976724, 0.7846976836063683791, 0.000000000000000000 ) ) ;
#7113 = DIRECTION ( 'NONE',  ( 0.000000000000000000, 0.000000000000000000, -1.000000000000000000 ) ) ;
#7114 = ORIENTED_EDGE ( 'NONE', *, *, #214, .T. ) ;
#7115 = DIRECTION ( 'NONE',  ( 0.000000000000000000, 0.000000000000000000, 1.000000000000000000 ) ) ;
#7116 = DIRECTION ( 'NONE',  ( -0.000000000000000000, -0.000000000000000000, -1.000000000000000000 ) ) ;
#7117 = EDGE_CURVE ( 'NONE', #6024, #7934, #4608, .T. ) ;
#7118 = CARTESIAN_POINT ( 'NONE',  ( 70.13889364076312916, -3.720050473604477936, 76.00117364557129918 ) ) ;
#7119 = CARTESIAN_POINT ( 'NONE',  ( -65.00000000000001421, -85.24929059928629727, -22.52499999999999503 ) ) ;
#7120 = VECTOR ( 'NONE', #1629, 1000.000000000000000 ) ;
#7121 = AXIS2_PLACEMENT_3D ( 'NONE', #8781, #13557, #4013 ) ;
#7122 = EDGE_CURVE ( 'NONE', #14307, #12689, #50, .T. ) ;
#7123 = ADVANCED_FACE ( 'NONE', ( #2507 ), #12558, .T. ) ;
#7124 = CARTESIAN_POINT ( 'NONE',  ( 23.36173033120691400, -85.24929059928631148, -6.000000000000000888 ) ) ;
#7125 = CARTESIAN_POINT ( 'NONE',  ( -24.91597137788995298, -6.538835002183793321, 48.06338840812244939 ) ) ;
#7126 = CARTESIAN_POINT ( 'NONE',  ( 14.23713579618830316, -69.39711819508849544, 4.406545790198910240 ) ) ;
#7127 = CARTESIAN_POINT ( 'NONE',  ( 33.32619986127557610, -54.90543917109370398, 2.016464562562223950 ) ) ;
#7128 = ORIENTED_EDGE ( 'NONE', *, *, #13338, .F. ) ;
#7129 = DIRECTION ( 'NONE',  ( 0.8746197071345569451, -0.4848096202550666312, 0.000000000000000000 ) ) ;
#7130 = ORIENTED_EDGE ( 'NONE', *, *, #1043, .F. ) ;
#7131 = CARTESIAN_POINT ( 'NONE',  ( 82.49066175147797253, 12.46743062497963450, -33.00000000000012790 ) ) ;
#7132 = AXIS2_PLACEMENT_3D ( 'NONE', #3716, #8424, #5811 ) ;
#7133 = ORIENTED_EDGE ( 'NONE', *, *, #6487, .T. ) ;
#7134 = VERTEX_POINT ( 'NONE', #11239 ) ;
#7135 = CARTESIAN_POINT ( 'NONE',  ( 65.32328153643977942, -11.87131781769073058, 75.71655242319833690 ) ) ;
#7136 = CARTESIAN_POINT ( 'NONE',  ( 80.00000000000001421, -72.24929059928631148, -32.99999999999999289 ) ) ;
#7137 = CARTESIAN_POINT ( 'NONE',  ( 23.47858629692700916, -53.24929059928630437, -6.492462156583981070 ) ) ;
#7138 = CARTESIAN_POINT ( 'NONE',  ( 8.090312502367355663, -56.83321641073667507, 1.823854045752810960 ) ) ;
#7139 = AXIS2_PLACEMENT_3D ( 'NONE', #7522, #8820, #4124 ) ;
#7140 = CARTESIAN_POINT ( 'NONE',  ( -16.99999999999998579, -2.249290599286303927, 50.00000000000012079 ) ) ;
#7141 = DIRECTION ( 'NONE',  ( -0.8420378618367728718, -0.5394184268574404584, -0.000000000000000000 ) ) ;
#7142 = VERTEX_POINT ( 'NONE', #2939 ) ;
#7143 = VERTEX_POINT ( 'NONE', #8777 ) ;
#7144 = PLANE ( 'NONE',  #5840 ) ;
#7145 = ORIENTED_EDGE ( 'NONE', *, *, #3568, .F. ) ;
#7146 = CARTESIAN_POINT ( 'NONE',  ( 38.02030736597991023, -69.39711819508849544, 2.500000000000000000 ) ) ;
#7147 = VERTEX_POINT ( 'NONE', #13626 ) ;
#7148 = DIRECTION ( 'NONE',  ( 0.5006040828730242698, -0.8656763553493063146, 0.000000000000000000 ) ) ;
#7149 = ORIENTED_EDGE ( 'NONE', *, *, #6358, .F. ) ;
#7150 = DIRECTION ( 'NONE',  ( -0.000000000000000000, 0.000000000000000000, -1.000000000000000000 ) ) ;
#7151 = CARTESIAN_POINT ( 'NONE',  ( -16.99999999999998579, 7.750709400713696517, 33.00000000000012790 ) ) ;
#7152 = EDGE_LOOP ( 'NONE', ( #8172, #10984, #13226, #12065, #15016 ) ) ;
#7153 = EDGE_CURVE ( 'NONE', #3379, #14082, #11998, .T. ) ;
#7154 = CARTESIAN_POINT ( 'NONE',  ( 20.86173033120691045, -87.24929059928631148, 3.999999999999999112 ) ) ;
#7155 = CARTESIAN_POINT ( 'NONE',  ( 70.08251421541277182, -3.500407835281747371, 72.53991591819000462 ) ) ;
#7156 = AXIS2_PLACEMENT_3D ( 'NONE', #7146, #9544, #7223 ) ;
#7157 = ORIENTED_EDGE ( 'NONE', *, *, #8646, .F. ) ;
#7158 = CIRCLE ( 'NONE', #6900, 2.499999999999995115 ) ;
#7159 = FACE_OUTER_BOUND ( 'NONE', #4496, .T. ) ;
#7160 = CARTESIAN_POINT ( 'NONE',  ( -9.394882438906904554, 2.563636819302931524, -48.00656353678737531 ) ) ;
#7161 = DIRECTION ( 'NONE',  ( -0.000000000000000000, 1.000000000000000000, -0.000000000000000000 ) ) ;
#7162 = ORIENTED_EDGE ( 'NONE', *, *, #10485, .T. ) ;
#7163 = CARTESIAN_POINT ( 'NONE',  ( 58.00000000000000711, -2.249290599286311032, 139.1143251403882459 ) ) ;
#7164 = EDGE_CURVE ( 'NONE', #1600, #7233, #5399, .T. ) ;
#7165 = ADVANCED_FACE ( 'NONE', ( #14706 ), #2000, .T. ) ;
#7166 = TOROIDAL_SURFACE ( 'NONE', #2250, 3.694885682588112452, 0.5000000000000000000 ) ;
#7167 = EDGE_LOOP ( 'NONE', ( #11484, #5134, #5295, #2696 ) ) ;
#7168 = CYLINDRICAL_SURFACE ( 'NONE', #7665, 0.7892041907098262810 ) ;
#7169 = EDGE_LOOP ( 'NONE', ( #5057, #11744, #2231, #12024 ) ) ;
#7170 = CIRCLE ( 'NONE', #14536, 0.9999999999999957812 ) ;
#7171 = CARTESIAN_POINT ( 'NONE',  ( 0.000000000000000000, 0.000000000000000000, 0.000000000000000000 ) ) ;
#7172 = FACE_OUTER_BOUND ( 'NONE', #8097, .T. ) ;
#7173 = CARTESIAN_POINT ( 'NONE',  ( 28.30879605499156781, -66.31562986446991204, 3.513916789801492246 ) ) ;
#7174 = CARTESIAN_POINT ( 'NONE',  ( -65.00000000000001421, -85.27429059928628874, -19.99999999999999645 ) ) ;
#7175 = DIRECTION ( 'NONE',  ( 1.000000000000000000, 1.156482317317870492E-16, 0.000000000000000000 ) ) ;
#7176=STYLED_ITEM('',(#15265),#14292);
#7177 = DIRECTION ( 'NONE',  ( 0.000000000000000000, 0.000000000000000000, 1.000000000000000000 ) ) ;
#7178 = CARTESIAN_POINT ( 'NONE',  ( -8.537170960192327129, 2.067018546614582508, 58.00000000000012079 ) ) ;
#7179 = VECTOR ( 'NONE', #13305, 1000.000000000000000 ) ;
#7180 = DIRECTION ( 'NONE',  ( 0.000000000000000000, 0.000000000000000000, 1.000000000000000000 ) ) ;
#7181 = AXIS2_PLACEMENT_3D ( 'NONE', #10622, #13160, #1305 ) ;
#7182 = VERTEX_POINT ( 'NONE', #14625 ) ;
#7183 = DIRECTION ( 'NONE',  ( 1.000000000000000000, 0.000000000000000000, 0.000000000000000000 ) ) ;
#7184 = ORIENTED_EDGE ( 'NONE', *, *, #6003, .F. ) ;
#7185 = CARTESIAN_POINT ( 'NONE',  ( 11.81495288376024533, -52.27629750527023589, -3.048923371196201160 ) ) ;
#7186 = CARTESIAN_POINT ( 'NONE',  ( 31.62070968671300975, -60.61174154192055141, -3.004298789847841267 ) ) ;
#7187 = VERTEX_POINT ( 'NONE', #8856 ) ;
#7188 = AXIS2_PLACEMENT_3D ( 'NONE', #7967, #6725, #6646 ) ;
#7189 = PLANE ( 'NONE',  #13827 ) ;
#7190 = CARTESIAN_POINT ( 'NONE',  ( 60.40269930420516431, 2.204737408716291647, 60.61639468829817190 ) ) ;
#7191 = CIRCLE ( 'NONE', #4466, 2.000000000000000000 ) ;
#7192 = ADVANCED_FACE ( 'NONE', ( #10174 ), #12325, .T. ) ;
#7193 = CIRCLE ( 'NONE', #545, 0.5000000000000000000 ) ;
#7194 = DIRECTION ( 'NONE',  ( -1.000000000000000000, -1.156482317317871478E-16, 0.000000000000000000 ) ) ;
#7195 = CARTESIAN_POINT ( 'NONE',  ( -24.96222495693456978, -7.431276100536581275, -58.00000000000012079 ) ) ;
#7196 = TOROIDAL_SURFACE ( 'NONE', #7441, 3.694885682588112452, 0.5000000000000000000 ) ;
#7197 = DIRECTION ( 'NONE',  ( 0.000000000000000000, 0.000000000000000000, -1.000000000000000000 ) ) ;
#7198 = DIRECTION ( 'NONE',  ( -0.000000000000000000, -1.000000000000000000, -0.000000000000000000 ) ) ;
#7199 = CARTESIAN_POINT ( 'NONE',  ( 30.00655632846217102, -52.27452423507310186, 4.068013018865621611 ) ) ;
#7200 = VERTEX_POINT ( 'NONE', #12038 ) ;
#7201 = AXIS2_PLACEMENT_3D ( 'NONE', #5999, #12924, #11756 ) ;
#7202 = PLANE ( 'NONE',  #7299 ) ;
#7203 = UNCERTAINTY_MEASURE_WITH_UNIT (LENGTH_MEASURE( 1.000000000000000082E-05 ), #14861, 'distance_accuracy_value', 'NONE');
#7204 = VERTEX_POINT ( 'NONE', #14781 ) ;
#7205 = DIRECTION ( 'NONE',  ( 0.000000000000000000, -1.000000000000000000, 0.000000000000000000 ) ) ;
#7206 = VERTEX_POINT ( 'NONE', #1849 ) ;
#7207 = ORIENTED_EDGE ( 'NONE', *, *, #4240, .T. ) ;
#7208 = CARTESIAN_POINT ( 'NONE',  ( 76.30169691776963248, -7.820670586471449859, 76.19766410831374515 ) ) ;
#7209 = DIRECTION ( 'NONE',  ( -0.8746197071345571672, 0.4848096202550659650, 0.000000000000000000 ) ) ;
#7210 = ADVANCED_FACE ( 'NONE', ( #11168 ), #9425, .F. ) ;
#7211 = ADVANCED_FACE ( 'NONE', ( #13938 ), #10630, .F. ) ;
#7212 = CARTESIAN_POINT ( 'NONE',  ( 13.86173033120691223, -69.39711819508849544, -3.619682905202625811 ) ) ;
#7213 = AXIS2_PLACEMENT_3D ( 'NONE', #3049, #6580, #3119 ) ;
#7214 = ORIENTED_EDGE ( 'NONE', *, *, #14373, .F. ) ;
#7215 = CIRCLE ( 'NONE', #3775, 2.524999999999999467 ) ;
#7216 = LINE ( 'NONE', #3748, #7940 ) ;
#7217 = CARTESIAN_POINT ( 'NONE',  ( -1.197457146693678753, -2.220571218158920335, 58.00000000000012079 ) ) ;
#7218 = ORIENTED_EDGE ( 'NONE', *, *, #9044, .F. ) ;
#7219 = EDGE_LOOP ( 'NONE', ( #7077, #6746, #2366, #7073 ) ) ;
#7220 = CARTESIAN_POINT ( 'NONE',  ( 64.94578693130894465, -11.37100417537640951, 76.92716210679893152 ) ) ;
#7221 = VERTEX_POINT ( 'NONE', #4465 ) ;
#7222 = ORIENTED_EDGE ( 'NONE', *, *, #7333, .F. ) ;
#7223 = DIRECTION ( 'NONE',  ( -1.000000000000000000, 0.000000000000000000, 0.000000000000000000 ) ) ;
#7224 = ORIENTED_EDGE ( 'NONE', *, *, #10388, .F. ) ;
#7225 = CARTESIAN_POINT ( 'NONE',  ( 14.46727374856319948, -52.24929059928630437, 3.946674197044067522 ) ) ;
#7226 = EDGE_CURVE ( 'NONE', #11898, #14830, #6774, .T. ) ;
#7227 = EDGE_LOOP ( 'NONE', ( #11761, #1984 ) ) ;
#7228 = CARTESIAN_POINT ( 'NONE',  ( 62.67308791069655882, 25.52935533987996664, 33.00000000000014211 ) ) ;
#7229 = LINE ( 'NONE', #9553, #6690 ) ;
#7230 = ORIENTED_EDGE ( 'NONE', *, *, #13831, .F. ) ;
#7231 = LINE ( 'NONE', #8474, #4721 ) ;
#7232 = LINE ( 'NONE', #11994, #12338 ) ;
#7233 = VERTEX_POINT ( 'NONE', #9403 ) ;
#7234 = DIRECTION ( 'NONE',  ( -1.000000000000000000, -1.156482317317870492E-16, 0.000000000000000000 ) ) ;
#7235 = DIRECTION ( 'NONE',  ( 1.224646799147353207E-16, -1.000000000000000000, 0.000000000000000000 ) ) ;
#7236 = DIRECTION ( 'NONE',  ( 0.000000000000000000, 0.000000000000000000, 1.000000000000000000 ) ) ;
#7237 = VERTEX_POINT ( 'NONE', #997 ) ;
#7238 = LINE ( 'NONE', #9999, #5869 ) ;
#7239 = B_SPLINE_CURVE_WITH_KNOTS ( 'NONE', 3,
 ( #11768, #83, #10695, #1223, #5931, #10616, #6920, #3610, #8321, #151, #2540, #11915 ),
 .UNSPECIFIED., .F., .F.,
 ( 4, 2, 2, 2, 2, 4 ),
 ( 0.000000000000000000, 0.001071381053236910479, 0.002142762106473820958, 0.003214143159710731654, 0.003749833686329185484, 0.004285524212947640181 ),
 .UNSPECIFIED. ) ;
#7240 = ORIENTED_EDGE ( 'NONE', *, *, #1237, .T. ) ;
#7241 = PLANE ( 'NONE',  #7443 ) ;
#7242 = SURFACE_STYLE_USAGE ( .BOTH. , #11629 ) ;
#7243 = EDGE_LOOP ( 'NONE', ( #8133, #3535, #12945, #7847 ) ) ;
#7244 = ORIENTED_EDGE ( 'NONE', *, *, #5245, .F. ) ;
#7245 = CARTESIAN_POINT ( 'NONE',  ( 8.333746554286330266, -58.06117559053658539, 1.821720188289711828 ) ) ;
#7246 = EDGE_CURVE ( 'NONE', #4595, #8405, #4838, .T. ) ;
#7247 = DIRECTION ( 'NONE',  ( -1.000000000000000000, 0.000000000000000000, 0.000000000000000000 ) ) ;
#7248 = CARTESIAN_POINT ( 'NONE',  ( -1.197457146693715613, -2.220571218158943871, -48.50000000000012079 ) ) ;
#7249 = VERTEX_POINT ( 'NONE', #14017 ) ;
#7250 = CARTESIAN_POINT ( 'NONE',  ( -2.688903428702175252E-15, 23.25070940071368142, 139.1143251403882459 ) ) ;
#7251 = EDGE_CURVE ( 'NONE', #3243, #3807, #7538, .T. ) ;
#7252 = EDGE_CURVE ( 'NONE', #14923, #13766, #9045, .T. ) ;
#7253 = EDGE_CURVE ( 'NONE', #5759, #7134, #11538, .T. ) ;
#7254 = CARTESIAN_POINT ( 'NONE',  ( 52.42117158417902800, -3.175556148104785592, 62.84860122826521689 ) ) ;
#7255 = CARTESIAN_POINT ( 'NONE',  ( 27.41706354086110053, -67.71210253279710400, 4.528315385689345440 ) ) ;
#7256 = CARTESIAN_POINT ( 'NONE',  ( -24.64146379341137560, -7.004861575982634037, 47.89606589046130125 ) ) ;
#7257 = FACE_OUTER_BOUND ( 'NONE', #9863, .T. ) ;
#7258 =( BOUNDED_SURFACE ( )  B_SPLINE_SURFACE ( 3, 2, ( 
 ( #10529, #14066, #12921 ),
 ( #5768, #11751, #8300 ),
 ( #9220, #12764, #13988 ),
 ( #15069, #6901, #8227 ) ),
 .UNSPECIFIED., .F., .F., .F. ) 
 B_SPLINE_SURFACE_WITH_KNOTS ( ( 4, 4 ),
 ( 3, 3 ),
 ( -5.204170427930421283E-18, 0.006683255761480927717 ),
 ( 0.000000000000000000, 1.000000000000000000 ),
 .UNSPECIFIED. ) 
 GEOMETRIC_REPRESENTATION_ITEM ( )  RATIONAL_B_SPLINE_SURFACE ( (
 ( 1.000000000000000000, 0.6947298545087535748, 1.000000000000000000),
 ( 1.000000000000000000, 0.6996284196041352432, 1.000000000000000000),
 ( 1.000000000000000000, 0.7035788727800805775, 1.000000000000000000),
 ( 1.000000000000000000, 0.7071067811865502373, 1.000000000000000000) ) ) 
 REPRESENTATION_ITEM ( '' )  SURFACE ( )  );
#7259 = EDGE_CURVE ( 'NONE', #6007, #7276, #3473, .T. ) ;
#7260 = FACE_OUTER_BOUND ( 'NONE', #1528, .T. ) ;
#7261 = VERTEX_POINT ( 'NONE', #7941 ) ;
#7262 = PRESENTATION_STYLE_ASSIGNMENT (( #7491 ) ) ;
#7263 = CARTESIAN_POINT ( 'NONE',  ( 31.74060919862615293, -60.49988549795170911, -2.962481358178278512 ) ) ;
#7264 = PLANE ( 'NONE',  #2392 ) ;
#7265 = CARTESIAN_POINT ( 'NONE',  ( 62.80358567007132820, -3.842053655357405173, 48.51982618741349285 ) ) ;
#7266 = CARTESIAN_POINT ( 'NONE',  ( 70.22816873311688823, -4.160343359009085695, 76.17259974762927754 ) ) ;
#7267 = CARTESIAN_POINT ( 'NONE',  ( 65.51779039507005109, -10.90589748781266799, 71.21143314006940273 ) ) ;
#7268 = EDGE_CURVE ( 'NONE', #9532, #3566, #2416, .T. ) ;
#7269 = CARTESIAN_POINT ( 'NONE',  ( 68.00000000000001421, 1.887379141862766624E-13, -33.00000000000012790 ) ) ;
#7270 = CARTESIAN_POINT ( 'NONE',  ( -20.99999999999998579, -2.249290599286303483, 38.00000000000012079 ) ) ;
#7271 = CIRCLE ( 'NONE', #5559, 0.4999999999999994449 ) ;
#7272 = EDGE_CURVE ( 'NONE', #6079, #13863, #7489, .T. ) ;
#7273 = CARTESIAN_POINT ( 'NONE',  ( 30.16594816474676222, -53.31348408104258851, 3.971884189131149157 ) ) ;
#7274 = VERTEX_POINT ( 'NONE', #2320 ) ;
#7275 = DIRECTION ( 'NONE',  ( -0.000000000000000000, 0.000000000000000000, -1.000000000000000000 ) ) ;
#7276 = VERTEX_POINT ( 'NONE', #15170 ) ;
#7277 = CARTESIAN_POINT ( 'NONE',  ( -16.99999999999998579, -2.249290599286303927, -57.50000000000012079 ) ) ;
#7278 = ORIENTED_EDGE ( 'NONE', *, *, #13558, .T. ) ;
#7279 = ORIENTED_EDGE ( 'NONE', *, *, #10225, .F. ) ;
#7280 = ORIENTED_EDGE ( 'NONE', *, *, #5225, .F. ) ;
#7281 = CARTESIAN_POINT ( 'NONE',  ( 64.91667272866463634, -11.40845216726351730, 75.99502765390730019 ) ) ;
#7282 = LINE ( 'NONE', #9755, #9010 ) ;
#7283 = DIRECTION ( 'NONE',  ( 0.8420378618367644341, 0.5394184268574535590, 0.000000000000000000 ) ) ;
#7284 = EDGE_CURVE ( 'NONE', #1809, #7515, #13, .T. ) ;
#7285 = CARTESIAN_POINT ( 'NONE',  ( 8.909806966310732435, -55.58532807872911263, 2.910983838681330926 ) ) ;
#7286 = CARTESIAN_POINT ( 'NONE',  ( -2.016677571526633510E-15, 23.25070940071368497, -33.00000000000012790 ) ) ;
#7287 = EDGE_CURVE ( 'NONE', #11327, #13307, #9715, .T. ) ;
#7288 = ADVANCED_FACE ( 'NONE', ( #12004 ), #1616, .F. ) ;
#7289 = DIRECTION ( 'NONE',  ( 1.000000000000000000, 0.000000000000000000, 0.000000000000000000 ) ) ;
#7290 = VECTOR ( 'NONE', #10371, 1000.000000000000000 ) ;
#7291 = ORIENTED_EDGE ( 'NONE', *, *, #4744, .F. ) ;
#7292 = ORIENTED_EDGE ( 'NONE', *, *, #11997, .T. ) ;
#7293 = VECTOR ( 'NONE', #948, 1000.000000000000000 ) ;
#7294 = DIRECTION ( 'NONE',  ( -1.000000000000000000, -8.673617379884035472E-17, 0.000000000000000000 ) ) ;
#7295 = VERTEX_POINT ( 'NONE', #10708 ) ;
#7296 = CARTESIAN_POINT ( 'NONE',  ( 32.14997420079631496, -58.98766849246937483, 1.832439066040240094 ) ) ;
#7297 = EDGE_LOOP ( 'NONE', ( #10654, #11777, #11698, #13745 ) ) ;
#7298 = CYLINDRICAL_SURFACE ( 'NONE', #8606, 0.5000000000000001110 ) ;
#7299 = AXIS2_PLACEMENT_3D ( 'NONE', #4747, #8510, #2509 ) ;
#7300 = EDGE_LOOP ( 'NONE', ( #831, #4689, #5338, #699 ) ) ;
#7301 = VECTOR ( 'NONE', #2495, 1000.000000000000000 ) ;
#7302 = DIRECTION ( 'NONE',  ( -0.000000000000000000, -1.000000000000000000, -0.000000000000000000 ) ) ;
#7303 = CARTESIAN_POINT ( 'NONE',  ( -16.99999999999998579, -2.249290599286303927, 58.00000000000012079 ) ) ;
#7304 = ORIENTED_EDGE ( 'NONE', *, *, #14674, .T. ) ;
#7305 = CARTESIAN_POINT ( 'NONE',  ( 23.69232253801246912, -85.24929059928631148, 4.472107801411126182 ) ) ;
#7306 = VECTOR ( 'NONE', #3722, 1000.000000000000000 ) ;
#7307 = VERTEX_POINT ( 'NONE', #14248 ) ;
#7308 = EDGE_CURVE ( 'NONE', #6214, #10074, #2620, .T. ) ;
#7309 = CARTESIAN_POINT ( 'NONE',  ( 42.07846078193830408, 0.000000000000000000, -33.00000000000012790 ) ) ;
#7310 = CARTESIAN_POINT ( 'NONE',  ( -21.58505662828840599, 4.908031226326156293, 57.50000000000012079 ) ) ;
#7311 = EDGE_CURVE ( 'NONE', #9911, #7744, #12085, .T. ) ;
#7312 = CARTESIAN_POINT ( 'NONE',  ( -3.190546569013415379, 0.8906624217387615339, 58.00000000000012079 ) ) ;
#7313 = ORIENTED_EDGE ( 'NONE', *, *, #11839, .T. ) ;
#7314 = DIRECTION ( 'NONE',  ( -0.000000000000000000, -0.000000000000000000, -1.000000000000000000 ) ) ;
#7315 = CIRCLE ( 'NONE', #10258, 9.000000000000001776 ) ;
#7316 = AXIS2_PLACEMENT_3D ( 'NONE', #3848, #7547, #13465 ) ;
#7317 = ORIENTED_EDGE ( 'NONE', *, *, #7691, .T. ) ;
#7318 = CARTESIAN_POINT ( 'NONE',  ( 33.02260275403471468, -59.65407802634348400, -1.835581805806632438 ) ) ;
#7319 = CARTESIAN_POINT ( 'NONE',  ( 69.44126955160255932, -2.986686531272439993, 71.69793282463490414 ) ) ;
#7320 = ORIENTED_EDGE ( 'NONE', *, *, #609, .T. ) ;
#7321 = PRODUCT_CONTEXT ( 'NONE', #13438, 'mechanical' ) ;
#7322 = FACE_OUTER_BOUND ( 'NONE', #5215, .T. ) ;
#7323 = FACE_OUTER_BOUND ( 'NONE', #2621, .T. ) ;
#7324 = CIRCLE ( 'NONE', #2657, 4.000000000000003553 ) ;
#7325 = CARTESIAN_POINT ( 'NONE',  ( -8.982583014919022446, 1.839844381040865562, -47.50000000000012079 ) ) ;
#7326 = CARTESIAN_POINT ( 'NONE',  ( 80.00000000000001421, -85.24929059928631148, -6.000000000000001776 ) ) ;
#7327 = AXIS2_PLACEMENT_3D ( 'NONE', #4813, #12727, #9107 ) ;
#7328 = CARTESIAN_POINT ( 'NONE',  ( 32.83279110308084370, -60.05631636466448242, 1.868376189747854577 ) ) ;
#7329 = DIRECTION ( 'NONE',  ( 0.000000000000000000, 1.000000000000000000, 0.000000000000000000 ) ) ;
#7330 = LINE ( 'NONE', #9733, #4656 ) ;
#7331 = CARTESIAN_POINT ( 'NONE',  ( 29.98602442760622822, -52.28438478636454789, 3.027705649770566332 ) ) ;
#7332 = CARTESIAN_POINT ( 'NONE',  ( 32.67588808858498339, -55.23312247377303663, -2.984220967394245694 ) ) ;
#7333 = EDGE_CURVE ( 'NONE', #4396, #8798, #5155, .T. ) ;
#7334 = DIRECTION ( 'NONE',  ( -1.000000000000000000, -1.156482317317870492E-16, 0.000000000000000000 ) ) ;
#7335 = ORIENTED_EDGE ( 'NONE', *, *, #264, .T. ) ;
#7336 = CARTESIAN_POINT ( 'NONE',  ( 53.34060950309435611, 1.272953934520814734, 48.51982618741349285 ) ) ;
#7337 = CARTESIAN_POINT ( 'NONE',  ( 23.55360291105710147, -55.94205978621073427, 6.462225911923646926 ) ) ;
#7338 = AXIS2_PLACEMENT_3D ( 'NONE', #917, #8086, #4699 ) ;
#7339 = ORIENTED_EDGE ( 'NONE', *, *, #4286, .T. ) ;
#7340 = DIRECTION ( 'NONE',  ( 1.000000000000000000, 0.000000000000000000, 0.000000000000000000 ) ) ;
#7341 = ORIENTED_EDGE ( 'NONE', *, *, #5328, .F. ) ;
#7342 = CARTESIAN_POINT ( 'NONE',  ( 69.46221311437308543, -2.886128739015260791, 75.19766410831374515 ) ) ;
#7343 = CARTESIAN_POINT ( 'NONE',  ( 104.9938193859979236, 23.25070940071369208, -33.00000000000012790 ) ) ;
#7344 = ADVANCED_FACE ( 'NONE', ( #10785 ), #10859, .F. ) ;
#7345 = EDGE_CURVE ( 'NONE', #5924, #13763, #9514, .T. ) ;
#7346 = CARTESIAN_POINT ( 'NONE',  ( 65.71319926014257362, -10.73129157630437902, 72.19766410831374515 ) ) ;
#7347 = DIRECTION ( 'NONE',  ( -0.8586863916854874379, 0.5125013958363018318, 0.000000000000000000 ) ) ;
#7348 =( BOUNDED_SURFACE ( )  B_SPLINE_SURFACE ( 3, 2, ( 
 ( #14561, #1634, #3023 ),
 ( #6334, #7713, #2715 ),
 ( #7557, #1568, #10955 ),
 ( #14626, #11026, #6480 ),
 ( #11169, #4078, #403 ),
 ( #1488, #478, #5104 ),
 ( #5255, #9811, #9952 ),
 ( #5402, #4468, #3607 ),
 ( #6625, #10095, #5718 ),
 ( #12635, #11463, #13713 ) ),
 .UNSPECIFIED., .F., .F., .F. ) 
 B_SPLINE_SURFACE_WITH_KNOTS ( ( 4, 2, 2, 2, 4 ),
 ( 3, 3 ),
 ( 0.0006711510808134562266, 0.001062132081067026709, 0.001453113081320596975, 0.001844094081574167241, 0.002235075081827737724 ),
 ( 0.000000000000000000, 1.000000000000000000 ),
 .UNSPECIFIED. ) 
 GEOMETRIC_REPRESENTATION_ITEM ( )  RATIONAL_B_SPLINE_SURFACE ( (
 ( 1.000000000000000000, 0.7254762501100212591, 1.000000000000000000),
 ( 1.000000000000000000, 0.7255094664176575670, 1.000000000000000000),
 ( 1.000000000000000000, 0.7239949553645330660, 1.000000000000000000),
 ( 1.000000000000000000, 0.7190573720639517052, 1.000000000000000000),
 ( 1.000000000000000000, 0.7156412189950384084, 1.000000000000000000),
 ( 1.000000000000000000, 0.7094102539595253942, 1.000000000000000000),
 ( 1.000000000000000000, 0.7066203625162220670, 1.000000000000000000),
 ( 1.000000000000000000, 0.7042417591948760824, 1.000000000000000000),
 ( 1.000000000000000000, 0.7046402682200600953, 1.000000000000000000),
 ( 1.000000000000000000, 0.7071067811865475727, 1.000000000000000000) ) ) 
 REPRESENTATION_ITEM ( '' )  SURFACE ( )  );
#7349 = FACE_BOUND ( 'NONE', #7227, .T. ) ;
#7350 = CARTESIAN_POINT ( 'NONE',  ( 69.46454297103568365, -2.294433329326446280, 73.05950274574442460 ) ) ;
#7351 = ORIENTED_EDGE ( 'NONE', *, *, #3105, .T. ) ;
#7352 = PLANE ( 'NONE',  #14264 ) ;
#7353 = ORIENTED_EDGE ( 'NONE', *, *, #1143, .F. ) ;
#7354 = ADVANCED_FACE ( 'NONE', ( #319 ), #3034, .F. ) ;
#7355 = CARTESIAN_POINT ( 'NONE',  ( 14.38963276113425138, -69.39711819508849544, -4.502057496415714510 ) ) ;
#7356 = ORIENTED_EDGE ( 'NONE', *, *, #4782, .F. ) ;
#7357 = EDGE_CURVE ( 'NONE', #556, #1600, #4370, .T. ) ;
#7358 = ORIENTED_EDGE ( 'NONE', *, *, #9516, .T. ) ;
#7360 = ORIENTED_EDGE ( 'NONE', *, *, #1858, .F. ) ;
#7359 = CARTESIAN_POINT ( 'NONE',  ( 50.01091543003727224, 0.000000000000000000, 139.1143251403882459 ) ) ;
#7361 = PLANE ( 'NONE',  #7545 ) ;
#7362 = AXIS2_PLACEMENT_3D ( 'NONE', #6112, #14111, #13112 ) ;
#7363 = AXIS2_PLACEMENT_3D ( 'NONE', #14493, #8636, #13481 ) ;
#7364 = DIRECTION ( 'NONE',  ( 0.000000000000000000, 0.000000000000000000, -1.000000000000000000 ) ) ;
#7365 = EDGE_LOOP ( 'NONE', ( #5538, #9211, #10592, #8935 ) ) ;
#7366 = CARTESIAN_POINT ( 'NONE',  ( 8.352106461623211686, -55.04126158147143144, 2.748788379872049603 ) ) ;
#7367 = LINE ( 'NONE', #7286, #1312 ) ;
#7368 = DIRECTION ( 'NONE',  ( 0.000000000000000000, 0.000000000000000000, 1.000000000000000000 ) ) ;
#7369 = AXIS2_PLACEMENT_3D ( 'NONE', #12037, #8141, #12849 ) ;
#7370 = VECTOR ( 'NONE', #4954, 1000.000000000000000 ) ;
#7371 = ORIENTED_EDGE ( 'NONE', *, *, #5659, .T. ) ;
#7372 = ORIENTED_EDGE ( 'NONE', *, *, #1068, .F. ) ;
#7373 = CARTESIAN_POINT ( 'NONE',  ( 65.22482032124671036, -11.15177368841987793, 77.09111985363571762 ) ) ;
#7374 = EDGE_LOOP ( 'NONE', ( #3795, #3883, #5891, #8525 ) ) ;
#7375 = ORIENTED_EDGE ( 'NONE', *, *, #2459, .F. ) ;
#7376 = DIRECTION ( 'NONE',  ( -0.8208219420614786266, 0.4549890321264269955, 0.3453061251629919726 ) ) ;
#7377 = ORIENTED_EDGE ( 'NONE', *, *, #3436, .F. ) ;
#7378 = DIRECTION ( 'NONE',  ( 0.000000000000000000, 0.000000000000000000, -1.000000000000000000 ) ) ;
#7379 = AXIS2_PLACEMENT_3D ( 'NONE', #4639, #7103, #108 ) ;
#7380 = ORIENTED_EDGE ( 'NONE', *, *, #9117, .F. ) ;
#7381 = CARTESIAN_POINT ( 'NONE',  ( 52.83848824477699679, -4.298675648159541396, 48.51982618741349285 ) ) ;
#7382 = CARTESIAN_POINT ( 'NONE',  ( -11.58528623411511305, -9.440246857018177451, 48.26816462195812818 ) ) ;
#7383 = ORIENTED_EDGE ( 'NONE', *, *, #3030, .F. ) ;
#7384 = EDGE_CURVE ( 'NONE', #4878, #3027, #7238, .T. ) ;
#7385 = VECTOR ( 'NONE', #8939, 1000.000000000000000 ) ;
#7386 = CARTESIAN_POINT ( 'NONE',  ( 28.23010146222003058, -64.93526722763056114, -4.251815205945953302 ) ) ;
#7387 = CARTESIAN_POINT ( 'NONE',  ( 58.00000000000000711, -2.249290599286309256, 60.61639468829817190 ) ) ;
#7388 = ORIENTED_EDGE ( 'NONE', *, *, #12717, .T. ) ;
#7389 = ADVANCED_FACE ( 'NONE', ( #8834 ), #13685, .F. ) ;
#7390 = CARTESIAN_POINT ( 'NONE',  ( 88.00000000000001421, 10.75070940071369208, -33.00000000000012790 ) ) ;
#7391 = DIRECTION ( 'NONE',  ( 0.000000000000000000, 0.000000000000000000, -1.000000000000000000 ) ) ;
#7392 = CARTESIAN_POINT ( 'NONE',  ( 21.74884261173415467, -85.24929059928631148, 6.000000000000001776 ) ) ;
#7393 = VERTEX_POINT ( 'NONE', #11152 ) ;
#7394 = CARTESIAN_POINT ( 'NONE',  ( 65.70833467347884493, -11.75568048844567848, 72.37168010940773399 ) ) ;
#7395 = VERTEX_POINT ( 'NONE', #14839 ) ;
#7396 = VERTEX_POINT ( 'NONE', #2840 ) ;
#7397 = CARTESIAN_POINT ( 'NONE',  ( 68.00000000000000000, 2.750709400713692965, 139.1143251403882459 ) ) ;
#7398 = VERTEX_POINT ( 'NONE', #8989 ) ;
#7399 = SHAPE_DEFINITION_REPRESENTATION ( #4693, #11466 ) ;
#7400 = CARTESIAN_POINT ( 'NONE',  ( 29.35555050496136431, -52.24929059928631148, 2.500000000000000000 ) ) ;
#7401 = CARTESIAN_POINT ( 'NONE',  ( 64.90552635791956959, 12.46743062497963450, 33.00000000000012790 ) ) ;
#7402 = EDGE_CURVE ( 'NONE', #12222, #965, #602, .T. ) ;
#7403 = DIRECTION ( 'NONE',  ( -0.000000000000000000, -0.000000000000000000, -1.000000000000000000 ) ) ;
#7404 = CIRCLE ( 'NONE', #746, 0.5000000000000004441 ) ;
#7405 = CARTESIAN_POINT ( 'NONE',  ( 12.86631187927720354, -53.69100233678929612, 4.215531945485751386 ) ) ;
#7406 = DIRECTION ( 'NONE',  ( 0.000000000000000000, 1.000000000000000000, -0.000000000000000000 ) ) ;
#7407 = CARTESIAN_POINT ( 'NONE',  ( 20.86173033120691045, -69.39711819508849544, 0.000000000000000000 ) ) ;
#7408 = CARTESIAN_POINT ( 'NONE',  ( 29.66826185475808586, -52.24929059928631148, -3.114712537284251237 ) ) ;
#7409 = PRODUCT_DEFINITION_SHAPE ( 'NONE', 'NONE',  #15230 ) ;
#7410 = CIRCLE ( 'NONE', #282, 4.665819364273509073 ) ;
#7411 = AXIS2_PLACEMENT_3D ( 'NONE', #2723, #1126, #9375 ) ;
#7412 = CIRCLE ( 'NONE', #4953, 0.9999999999999977796 ) ;
#7413 = DIRECTION ( 'NONE',  ( 0.000000000000000000, 0.000000000000000000, 1.000000000000000000 ) ) ;
#7414 = ORIENTED_EDGE ( 'NONE', *, *, #5480, .T. ) ;
#7415 = DIRECTION ( 'NONE',  ( 1.000000000000000000, 0.000000000000000000, 0.000000000000000000 ) ) ;
#7416 = CARTESIAN_POINT ( 'NONE',  ( 33.12442989620986822, -59.21224831720010684, -1.832439066040426834 ) ) ;
#7417 = EDGE_CURVE ( 'NONE', #1375, #922, #13612, .T. ) ;
#7418 = DIRECTION ( 'NONE',  ( -0.000000000000000000, -1.000000000000000000, -0.000000000000000000 ) ) ;
#7419 = DIRECTION ( 'NONE',  ( -0.8746197071345569451, 0.4848096202550666312, 0.000000000000000000 ) ) ;
#7420 = CARTESIAN_POINT ( 'NONE',  ( 69.45904386152527366, -2.940328655257759216, 75.56077421381992565 ) ) ;
#7421 = AXIS2_PLACEMENT_3D ( 'NONE', #2858, #10957, #1411 ) ;
#7422 = CARTESIAN_POINT ( 'NONE',  ( 65.03642989375747163, -11.30142140009759544, 71.40617678772515831 ) ) ;
#7423 = VECTOR ( 'NONE', #10621, 1000.000000000000000 ) ;
#7424 = VECTOR ( 'NONE', #6017, 1000.000000000000000 ) ;
#7425 = PLANE ( 'NONE',  #15010 ) ;
#7426 = DIRECTION ( 'NONE',  ( 0.000000000000000000, 0.000000000000000000, 1.000000000000000000 ) ) ;
#7427 = ADVANCED_FACE ( 'NONE', ( #1760 ), #3145, .T. ) ;
#7428 = ORIENTED_EDGE ( 'NONE', *, *, #10960, .F. ) ;
#7429 = DIRECTION ( 'NONE',  ( 0.000000000000000000, 0.000000000000000000, 1.000000000000000000 ) ) ;
#7430 = CIRCLE ( 'NONE', #13562, 1.000000000000002665 ) ;
#7431 = AXIS2_PLACEMENT_3D ( 'NONE', #13845, #3378, #9232 ) ;
#7432 = VERTEX_POINT ( 'NONE', #14757 ) ;
#7433 = CARTESIAN_POINT ( 'NONE',  ( 17.61519226005271577, -69.39711819508866597, -6.201611931792120558 ) ) ;
#7434 = CARTESIAN_POINT ( 'NONE',  ( 19.97461805067967333, -85.24929059928631148, 4.000000000000001776 ) ) ;
#7435 = VECTOR ( 'NONE', #467, 1000.000000000000000 ) ;
#7436 = VERTEX_POINT ( 'NONE', #827 ) ;
#7437 = ORIENTED_EDGE ( 'NONE', *, *, #14754, .F. ) ;
#7439 = EDGE_LOOP ( 'NONE', ( #4437, #10993, #5521, #13882 ) ) ;
#7438 = LINE ( 'NONE', #13417, #6222 ) ;
#7440 = CARTESIAN_POINT ( 'NONE',  ( 58.00000000000000711, -2.249290599286309256, 82.40005259842790508 ) ) ;
#7441 = AXIS2_PLACEMENT_3D ( 'NONE', #7463, #14465, #3908 ) ;
#7442 = LINE ( 'NONE', #1438, #560 ) ;
#7443 = AXIS2_PLACEMENT_3D ( 'NONE', #11929, #8552, #13252 ) ;
#7444 = CARTESIAN_POINT ( 'NONE',  ( 8.134050929208209268, -55.84353942689834582, 1.893207994801671790 ) ) ;
#7445 = ADVANCED_FACE ( 'NONE', ( #1906 ), #4288, .F. ) ;
#7446 = EDGE_CURVE ( 'NONE', #8969, #1527, #5380, .T. ) ;
#7447 = EDGE_CURVE ( 'NONE', #13057, #3099, #10034, .T. ) ;
#7448 = DIRECTION ( 'NONE',  ( -1.000000000000000000, -8.673617379884035472E-17, 0.000000000000000000 ) ) ;
#7449 = DIRECTION ( 'NONE',  ( 0.000000000000000000, 0.000000000000000000, 1.000000000000000000 ) ) ;
#7450 = AXIS2_PLACEMENT_3D ( 'NONE', #9373, #63, #10372 ) ;
#7451 = VERTEX_POINT ( 'NONE', #12229 ) ;
#7452 = ORIENTED_EDGE ( 'NONE', *, *, #14436, .F. ) ;
#7453 = LINE ( 'NONE', #1369, #10000 ) ;
#7454 = ORIENTED_EDGE ( 'NONE', *, *, #10104, .T. ) ;
#7455 = EDGE_LOOP ( 'NONE', ( #4107, #7128 ) ) ;
#7456 = EDGE_CURVE ( 'NONE', #14789, #10204, #3400, .T. ) ;
#7457 = CARTESIAN_POINT ( 'NONE',  ( -22.13891797369473480, 5.141277655368648780, 48.38337049880507834 ) ) ;
#7458 = ORIENTED_EDGE ( 'NONE', *, *, #6712, .F. ) ;
#7459 = CARTESIAN_POINT ( 'NONE',  ( 58.00000000000000711, -2.249290599286309256, 76.19766410831374515 ) ) ;
#7460 = ORIENTED_EDGE ( 'NONE', *, *, #5963, .F. ) ;
#7461 = CIRCLE ( 'NONE', #4757, 2.000000000000000000 ) ;
#7462 = CARTESIAN_POINT ( 'NONE',  ( -2.016677571526633510E-15, 23.25070940071368497, 139.1143251403882459 ) ) ;
#7463 = CARTESIAN_POINT ( 'NONE',  ( -30.80945343098651890, -5.389243620311580329, 57.50000000000012079 ) ) ;
#7464 = ORIENTED_EDGE ( 'NONE', *, *, #11719, .F. ) ;
#7465 = VECTOR ( 'NONE', #1833, 1000.000000000000000 ) ;
#7466 = CARTESIAN_POINT ( 'NONE',  ( 28.79421079956400931, -63.81378734512018269, -4.043274055230903663 ) ) ;
#7467 = VERTEX_POINT ( 'NONE', #5304 ) ;
#7468 = DIRECTION ( 'NONE',  ( 0.000000000000000000, 0.000000000000000000, -1.000000000000000000 ) ) ;
#7469 = DIRECTION ( 'NONE',  ( 1.000000000000000000, 0.000000000000000000, 0.000000000000000000 ) ) ;
#7470 = LINE ( 'NONE', #14837, #5014 ) ;
#7471 = ORIENTED_EDGE ( 'NONE', *, *, #14754, .T. ) ;
#7472 = ORIENTED_EDGE ( 'NONE', *, *, #4629, .T. ) ;
#7473 = CARTESIAN_POINT ( 'NONE',  ( -21.85476584171706449, 5.329050157244581420, 48.50000000000012079 ) ) ;
#7474 = EDGE_LOOP ( 'NONE', ( #2143, #12511, #14303, #7857 ) ) ;
#7475 = AXIS2_PLACEMENT_3D ( 'NONE', #7603, #5143, #377 ) ;
#7476 = ORIENTED_EDGE ( 'NONE', *, *, #9501, .T. ) ;
#7477 = DIRECTION ( 'NONE',  ( -0.8746197071345569451, 0.4848096202550666312, 0.000000000000000000 ) ) ;
#7478 = APPLICATION_PROTOCOL_DEFINITION ( 'draft international standard', 'automotive_design', 1998, #5959 ) ;
#7479 = CARTESIAN_POINT ( 'NONE',  ( 58.00000000000000711, -2.249290599286309256, 87.40005259842790508 ) ) ;
#7480 = LINE ( 'NONE', #1768, #12106 ) ;
#7481 = CARTESIAN_POINT ( 'NONE',  ( 66.92402464212069901, -2.249290599286309256, 39.50000000000012790 ) ) ;
#7482 = CARTESIAN_POINT ( 'NONE',  ( 18.10076659937403676, -57.98711502979269028, 6.432599168432305170 ) ) ;
#7483 = CARTESIAN_POINT ( 'NONE',  ( 56.28732689558331259, 3.089731932287651084, 48.51982618741349285 ) ) ;
#7484 = CARTESIAN_POINT ( 'NONE',  ( 33.58398609825992054, -55.86841147293986864, 1.893102220090065568 ) ) ;
#7485 = CARTESIAN_POINT ( 'NONE',  ( 13.77965687262189576, -67.87804980504300545, -4.252496648640687660 ) ) ;
#7486 = EDGE_CURVE ( 'NONE', #8402, #4620, #9861, .T. ) ;
#7487 = ADVANCED_FACE ( 'NONE', ( #6383 ), #5231, .F. ) ;
#7488 = DIRECTION ( 'NONE',  ( 1.000000000000000000, 0.000000000000000000, 0.000000000000000000 ) ) ;
#7489 = B_SPLINE_CURVE_WITH_KNOTS ( 'NONE', 3,
 ( #4628, #9323, #8174, #12877 ),
 .UNSPECIFIED., .F., .F.,
 ( 4, 4 ),
 ( 0.000000000000000000, 0.006683255761480919911 ),
 .UNSPECIFIED. ) ;
#7490 = VERTEX_POINT ( 'NONE', #4138 ) ;
#7491 = SURFACE_STYLE_USAGE ( .BOTH. , #5106 ) ;
#7492 = CARTESIAN_POINT ( 'NONE',  ( 47.27423575335444639, 25.52935533987996664, -33.00000000000012790 ) ) ;
#7493 = CARTESIAN_POINT ( 'NONE',  ( 58.00000000000000711, -2.249290599286309256, 39.50000000000012790 ) ) ;
#7494 = CARTESIAN_POINT ( 'NONE',  ( -80.00000000000001421, -85.24929059928629727, -8.000000000000001776 ) ) ;
#7495 = DIRECTION ( 'NONE',  ( -0.000000000000000000, 1.000000000000000000, -1.927470528863119788E-16 ) ) ;
#7496 = DIRECTION ( 'NONE',  ( 1.110223024625156540E-15, -1.000000000000000000, 0.000000000000000000 ) ) ;
#7497 = DIRECTION ( 'NONE',  ( -0.8746197071345572782, 0.4848096202550659650, 0.000000000000000000 ) ) ;
#7498 = EDGE_CURVE ( 'NONE', #3333, #11665, #6678, .T. ) ;
#7499 = EDGE_CURVE ( 'NONE', #12860, #11933, #1183, .T. ) ;
#7500 = ORIENTED_EDGE ( 'NONE', *, *, #3115, .T. ) ;
#7501 = DIRECTION ( 'NONE',  ( 0.000000000000000000, 0.000000000000000000, 1.000000000000000000 ) ) ;
#7502 = ORIENTED_EDGE ( 'NONE', *, *, #5283, .F. ) ;
#7503 = CARTESIAN_POINT ( 'NONE',  ( 0.000000000000000000, 21.75070940071309167, -33.00000000000012790 ) ) ;
#7504 = CARTESIAN_POINT ( 'NONE',  ( 65.00000000000001421, -85.24929059928629727, -22.52499999999999503 ) ) ;
#7505 = EDGE_LOOP ( 'NONE', ( #1598, #3624, #9389, #13880, #7769, #1356, #14217, #9768, #10761, #14873, #12093, #1509, #12343, #5562, #5206, #8580 ) ) ;
#7506 = CARTESIAN_POINT ( 'NONE',  ( -9.090012166261184134, -7.380334305945262408, 48.00000000000014211 ) ) ;
#7507 = DIRECTION ( 'NONE',  ( -1.000000000000000000, 0.000000000000000000, 0.000000000000000000 ) ) ;
#7508 = ORIENTED_EDGE ( 'NONE', *, *, #8496, .T. ) ;
#7509 = LINE ( 'NONE', #2816, #8447 ) ;
#7510 = VECTOR ( 'NONE', #12955, 1000.000000000000000 ) ;
#7511 = DIRECTION ( 'NONE',  ( 0.000000000000000000, 0.000000000000000000, 1.000000000000000000 ) ) ;
#7512 = DIRECTION ( 'NONE',  ( 0.000000000000000000, 1.000000000000000000, 0.000000000000000000 ) ) ;
#7513 =( REPRESENTATION_RELATIONSHIP ('NONE','NONE', #15125, #1557 ) REPRESENTATION_RELATIONSHIP_WITH_TRANSFORMATION ( #2782 )SHAPE_REPRESENTATION_RELATIONSHIP( ) );
#7514 = CARTESIAN_POINT ( 'NONE',  ( 80.00000000000001421, -85.24929059928631148, -6.000000000000001776 ) ) ;
#7515 = VERTEX_POINT ( 'NONE', #2918 ) ;
#7516 = ORIENTED_EDGE ( 'NONE', *, *, #1175, .F. ) ;
#7517 = CARTESIAN_POINT ( 'NONE',  ( 13.86173033120691223, -69.39711819508849544, 2.500000000000000000 ) ) ;
#7518 = EDGE_CURVE ( 'NONE', #7767, #4878, #6604, .T. ) ;
#7519 = ORIENTED_EDGE ( 'NONE', *, *, #12555, .F. ) ;
#7520 = DIRECTION ( 'NONE',  ( 0.000000000000000000, -0.000000000000000000, -1.000000000000000000 ) ) ;
#7521 = VERTEX_POINT ( 'NONE', #11291 ) ;
#7522 = CARTESIAN_POINT ( 'NONE',  ( 118.5627027169299765, -35.81974489651393156, 54.40673322733725570 ) ) ;
#7523 = VECTOR ( 'NONE', #2011, 1000.000000000000000 ) ;
#7524 = ORIENTED_EDGE ( 'NONE', *, *, #6976, .T. ) ;
#7525 = FACE_OUTER_BOUND ( 'NONE', #13703, .T. ) ;
#7526 = PLANE ( 'NONE',  #11859 ) ;
#7527 = ORIENTED_EDGE ( 'NONE', *, *, #12699, .F. ) ;
#7528 = CARTESIAN_POINT ( 'NONE',  ( 27.55953187330915810, 21.75070940071309167, -33.00000000000012790 ) ) ;
#7529 = ORIENTED_EDGE ( 'NONE', *, *, #2174, .F. ) ;
#7530 = ADVANCED_FACE ( 'NONE', ( #673 ), #7817, .T. ) ;
#7531 = CONICAL_SURFACE ( 'NONE', #10770, 2.524999999999999467, 0.7853981633973787790 ) ;
#7532 = AXIS2_PLACEMENT_3D ( 'NONE', #2290, #5836, #8060 ) ;
#7533 = DIRECTION ( 'NONE',  ( 0.8656763553492754504, 0.5006040828730772274, -1.896095000761754519E-14 ) ) ;
#7534 = CARTESIAN_POINT ( 'NONE',  ( 109.8334623555409735, 21.75070940071366365, 13.14990448602693007 ) ) ;
#7535 = DIRECTION ( 'NONE',  ( 0.8420378618367727608, 0.5394184268574406804, 0.000000000000000000 ) ) ;
#7536 = ORIENTED_EDGE ( 'NONE', *, *, #11367, .F. ) ;
#7537 = DIRECTION ( 'NONE',  ( 0.000000000000000000, 0.000000000000000000, 1.000000000000000000 ) ) ;
#7538 = CIRCLE ( 'NONE', #10528, 1.000000000000000000 ) ;
#7539 = ORIENTED_EDGE ( 'NONE', *, *, #11573, .T. ) ;
#7540 = ORIENTED_EDGE ( 'NONE', *, *, #1810, .F. ) ;
#7541 = EDGE_CURVE ( 'NONE', #10777, #3027, #5458, .T. ) ;
#7542 = CARTESIAN_POINT ( 'NONE',  ( 32.35376478511743414, -60.81027516727737492, -1.970305681586464130 ) ) ;
#7543 = VECTOR ( 'NONE', #2498, 1000.000000000000000 ) ;
#7544 = EDGE_CURVE ( 'NONE', #4976, #9584, #215, .T. ) ;
#7545 = AXIS2_PLACEMENT_3D ( 'NONE', #7136, #11820, #6220 ) ;
#7546 = APPLICATION_PROTOCOL_DEFINITION ( 'draft international standard', 'automotive_design', 1998, #857 ) ;
#7547 = DIRECTION ( 'NONE',  ( 0.000000000000000000, 0.000000000000000000, 1.000000000000000000 ) ) ;
#7548 = DIRECTION ( 'NONE',  ( 0.000000000000000000, 0.000000000000000000, 1.000000000000000000 ) ) ;
#7549 = DIRECTION ( 'NONE',  ( 0.8746197071345571672, -0.4848096202550661316, 0.000000000000000000 ) ) ;
#7550 = CARTESIAN_POINT ( 'NONE',  ( 9.124894037265468327, -59.08346394662398637, 2.725125706442365292 ) ) ;
#7551 = VECTOR ( 'NONE', #11502, 1000.000000000000000 ) ;
#7552 = DIRECTION ( 'NONE',  ( 0.000000000000000000, 0.000000000000000000, 1.000000000000000000 ) ) ;
#7553 = CIRCLE ( 'NONE', #909, 4.000000000000003553 ) ;
#7554 = DIRECTION ( 'NONE',  ( -1.156482317317870492E-16, 1.000000000000000000, -0.000000000000000000 ) ) ;
#7555 = LINE ( 'NONE', #1704, #4158 ) ;
#7556 = TOROIDAL_SURFACE ( 'NONE', #2879, 5.165819364273509073, 0.5000000000000000000 ) ;
#7557 = CARTESIAN_POINT ( 'NONE',  ( -9.443282642412393457, 2.639297360524499592, 48.23807154671105479 ) ) ;
#7558 = ORIENTED_EDGE ( 'NONE', *, *, #6773, .F. ) ;
#7559 = CARTESIAN_POINT ( 'NONE',  ( -80.00000000000001421, -74.24929059928631148, 4.000000000000000000 ) ) ;
#7560 = CARTESIAN_POINT ( 'NONE',  ( 54.00000000000000711, -2.249290599286310588, -38.00000000000012079 ) ) ;
#7561 = CARTESIAN_POINT ( 'NONE',  ( 50.19487218104683990, 2.077162398607073079, 39.50000000000012790 ) ) ;
#7562 = ORIENTED_EDGE ( 'NONE', *, *, #12949, .F. ) ;
#7563 = VECTOR ( 'NONE', #1330, 1000.000000000000000 ) ;
#7564 = CIRCLE ( 'NONE', #9262, 1.000000000000000888 ) ;
#7565 = DIRECTION ( 'NONE',  ( -0.000000000000000000, 0.000000000000000000, -1.000000000000000000 ) ) ;
#7566 = DIRECTION ( 'NONE',  ( 0.000000000000000000, 0.000000000000000000, 1.000000000000000000 ) ) ;
#7567 = EDGE_CURVE ( 'NONE', #5252, #13534, #11440, .T. ) ;
#7568 = DIRECTION ( 'NONE',  ( 0.000000000000000000, 0.000000000000000000, -1.000000000000000000 ) ) ;
#7569 = DIRECTION ( 'NONE',  ( -1.000000000000000000, 0.000000000000000000, 0.000000000000000000 ) ) ;
#7570 = CARTESIAN_POINT ( 'NONE',  ( 27.86173033120691045, -69.39711819508849544, -3.619682905202609380 ) ) ;
#7571 = AXIS2_PLACEMENT_3D ( 'NONE', #3577, #2581, #9279 ) ;
#7572 = ORIENTED_EDGE ( 'NONE', *, *, #11198, .F. ) ;
#7573 = CARTESIAN_POINT ( 'NONE',  ( 33.43681684131585996, -55.00297582962931386, -2.730999879046705825 ) ) ;
#7574 = ORIENTED_EDGE ( 'NONE', *, *, #12675, .T. ) ;
#7575 = CARTESIAN_POINT ( 'NONE',  ( 114.6731053250840233, 23.25070940071369563, 139.1143251403882459 ) ) ;
#7576 = DIRECTION ( 'NONE',  ( -0.000000000000000000, -0.000000000000000000, 1.000000000000000000 ) ) ;
#7577 = ORIENTED_EDGE ( 'NONE', *, *, #10069, .F. ) ;
#7579 = ORIENTED_EDGE ( 'NONE', *, *, #5378, .F. ) ;
#7578 = CARTESIAN_POINT ( 'NONE',  ( -80.00000000000001421, -85.24929059928629727, 32.00000000000000000 ) ) ;
#7580 = CARTESIAN_POINT ( 'NONE',  ( 14.09536732513642932, -69.39711819508849544, -4.287213148048568456 ) ) ;
#7581 = EDGE_LOOP ( 'NONE', ( #3717, #204, #2046, #4139 ) ) ;
#7582 = EDGE_CURVE ( 'NONE', #5046, #981, #5615, .T. ) ;
#7583 = ADVANCED_FACE ( 'NONE', ( #12688 ), #3454, .T. ) ;
#7584 = CARTESIAN_POINT ( 'NONE',  ( 10.87912556056369873, -61.22098757970047700, 3.286659897586142076 ) ) ;
#7585 = PRODUCT_DEFINITION ( 'UNKNOWN', '', #3869, #1353 ) ;
#7586 = ORIENTED_EDGE ( 'NONE', *, *, #4527, .F. ) ;
#7587 = CARTESIAN_POINT ( 'NONE',  ( 10.53962429902219000, -53.65556550047445228, 3.599583915703609804 ) ) ;
#7588 = VECTOR ( 'NONE', #14537, 1000.000000000000000 ) ;
#7589 = DIRECTION ( 'NONE',  ( 0.2245716668862471066, 0.9744202983869689749, -0.008523410314122858294 ) ) ;
#7590 = DIRECTION ( 'NONE',  ( -1.000000000000000000, 0.000000000000000000, -0.000000000000000000 ) ) ;
#7591 = ORIENTED_EDGE ( 'NONE', *, *, #8292, .F. ) ;
#7592 = ORIENTED_EDGE ( 'NONE', *, *, #395, .F. ) ;
#7593 = CARTESIAN_POINT ( 'NONE',  ( 9.541851365446024857, -61.03551305047443520, 2.732671606846408974 ) ) ;
#7594 = ORIENTED_EDGE ( 'NONE', *, *, #9956, .F. ) ;
#7595 = AXIS2_PLACEMENT_3D ( 'NONE', #14556, #7552, #12320 ) ;
#7596 = DIRECTION ( 'NONE',  ( 0.8208219420614786266, -0.4549890321264269955, -0.3453061251629919726 ) ) ;
#7597 = ORIENTED_EDGE ( 'NONE', *, *, #12152, .F. ) ;
#7598 = FACE_OUTER_BOUND ( 'NONE', #3831, .T. ) ;
#7599 = DIRECTION ( 'NONE',  ( -0.000000000000000000, -0.000000000000000000, -1.000000000000000000 ) ) ;
#7600 = ORIENTED_EDGE ( 'NONE', *, *, #2199, .F. ) ;
#7601 = ADVANCED_FACE ( 'NONE', ( #2139 ), #7747, .T. ) ;
#7602 = CARTESIAN_POINT ( 'NONE',  ( -25.99999999999998934, -2.249290599286303927, 47.50000000000012079 ) ) ;
#7603 = CARTESIAN_POINT ( 'NONE',  ( 54.03086304124234829, 0.8903401505190762233, 60.61639468829817190 ) ) ;
#7604 = ORIENTED_EDGE ( 'NONE', *, *, #6227, .F. ) ;
#7605 = CARTESIAN_POINT ( 'NONE',  ( 30.59344312246520659, -62.42480215138119348, -2.585081138714962368 ) ) ;
#7606 = VERTEX_POINT ( 'NONE', #11521 ) ;
#7607 = VECTOR ( 'NONE', #2060, 1000.000000000000114 ) ;
#7608 = AXIS2_PLACEMENT_3D ( 'NONE', #1181, #12893, #11554 ) ;
#7609 = CARTESIAN_POINT ( 'NONE',  ( 57.51704887355756313, 3.283153786997079049, 54.56811043785582882 ) ) ;
#7610 = CARTESIAN_POINT ( 'NONE',  ( 0.000000000000000000, 21.75070940071322667, -33.00000000000012790 ) ) ;
#7611 = DIRECTION ( 'NONE',  ( 0.000000000000000000, -0.000000000000000000, -1.000000000000000000 ) ) ;
#7612 = DIRECTION ( 'NONE',  ( 0.000000000000000000, 0.000000000000000000, 1.000000000000000000 ) ) ;
#7613 = VERTEX_POINT ( 'NONE', #3375 ) ;
#7614 = DIRECTION ( 'NONE',  ( -0.000000000000000000, -1.000000000000000000, -0.000000000000000000 ) ) ;
#7615 = ORIENTED_EDGE ( 'NONE', *, *, #12821, .F. ) ;
#7616 = EDGE_LOOP ( 'NONE', ( #6831, #9934, #14838, #6683 ) ) ;
#7617 = ORIENTED_EDGE ( 'NONE', *, *, #5696, .F. ) ;
#7618 = DIRECTION ( 'NONE',  ( 0.000000000000000000, 1.000000000000000000, 0.000000000000000000 ) ) ;
#7619 = EDGE_CURVE ( 'NONE', #9598, #2535, #2066, .T. ) ;
#7620 = TOROIDAL_SURFACE ( 'NONE', #486, 3.694885682587998765, 0.5000000000000000000 ) ;
#7621 = CARTESIAN_POINT ( 'NONE',  ( 10.23047706855496841, -60.71197230342421136, 3.050751728647412175 ) ) ;
#7622 = DIRECTION ( 'NONE',  ( 1.000000000000000000, 0.000000000000000000, 0.000000000000000000 ) ) ;
#7623 = CARTESIAN_POINT ( 'NONE',  ( 8.741688182926928619, -56.83166877439235520, -2.758334070755373624 ) ) ;
#7624 = VERTEX_POINT ( 'NONE', #15149 ) ;
#7625 = CARTESIAN_POINT ( 'NONE',  ( 51.75774672102440377, 0.000000000000000000, 33.00000000000012790 ) ) ;
#7626 = CARTESIAN_POINT ( 'NONE',  ( 65.08771336141364827, -11.27259367992862416, 72.26839924292039541 ) ) ;
#7627 = CARTESIAN_POINT ( 'NONE',  ( 51.75774672102440377, 0.000000000000000000, -33.00000000000012790 ) ) ;
#7628 = ADVANCED_FACE ( 'NONE', ( #4445 ), #10779, .T. ) ;
#7629 = DIRECTION ( 'NONE',  ( 0.000000000000000000, 0.000000000000000000, 1.000000000000000000 ) ) ;
#7630 = TOROIDAL_SURFACE ( 'NONE', #11551, 3.694885682587998765, 0.5000000000000000000 ) ;
#7631 = CARTESIAN_POINT ( 'NONE',  ( 13.86157779355430186, -69.45278782524461292, -3.616934341765148719 ) ) ;
#7632 = EDGE_CURVE ( 'NONE', #864, #10987, #1437, .T. ) ;
#7633 = ORIENTED_EDGE ( 'NONE', *, *, #3302, .T. ) ;
#7634 = DIRECTION ( 'NONE',  ( 0.8656763553493062036, 0.5006040828730242698, 0.000000000000000000 ) ) ;
#7635 = PLANE ( 'NONE',  #982 ) ;
#7636 = EDGE_LOOP ( 'NONE', ( #1982, #2065, #4588, #9428 ) ) ;
#7637 = CARTESIAN_POINT ( 'NONE',  ( 29.25823701260754817, -63.07964102605458123, -3.871020209143769097 ) ) ;
#7638 = DIRECTION ( 'NONE',  ( 1.000000000000000000, 8.673617379884035472E-17, 0.000000000000000000 ) ) ;
#7639 = EDGE_CURVE ( 'NONE', #5697, #8736, #11683, .T. ) ;
#7640 = AXIS2_PLACEMENT_3D ( 'NONE', #11286, #743, #12377 ) ;
#7641 = CARTESIAN_POINT ( 'NONE',  ( -80.00000000000001421, -87.24929059928631148, -35.00000000000000000 ) ) ;
#7642 = ORIENTED_EDGE ( 'NONE', *, *, #7059, .F. ) ;
#7643 = CARTESIAN_POINT ( 'NONE',  ( 8.989056138305015153, -55.35059346084328524, 2.955710789589967913 ) ) ;
#7644 = ADVANCED_FACE ( 'NONE', ( #1134 ), #10382, .T. ) ;
#7645 = AXIS2_PLACEMENT_3D ( 'NONE', #11369, #10384, #9071 ) ;
#7646 = FACE_OUTER_BOUND ( 'NONE', #12487, .T. ) ;
#7647 = CARTESIAN_POINT ( 'NONE',  ( 27.86173033120691045, -69.39711819508849544, 0.000000000000000000 ) ) ;
#7648 = CARTESIAN_POINT ( 'NONE',  ( -25.22031829551916360, -6.987901215495521789, -48.36903577193041315 ) ) ;
#7649 = COLOUR_RGB ( '',0.7921568627450980005, 0.8196078431372548767, 0.9333333333333333481 ) ;
#7650 = VECTOR ( 'NONE', #2616, 1000.000000000000000 ) ;
#7651 = VERTEX_POINT ( 'NONE', #5850 ) ;
#7652 = CARTESIAN_POINT ( 'NONE',  ( 23.62269406304343988, -57.98711502976567544, -6.432599168430717995 ) ) ;
#7653 = EDGE_CURVE ( 'NONE', #3003, #2288, #10538, .T. ) ;
#7654 = VERTEX_POINT ( 'NONE', #9069 ) ;
#7655 = DIRECTION ( 'NONE',  ( -0.000000000000000000, -0.000000000000000000, -1.000000000000000000 ) ) ;
#7656 = CARTESIAN_POINT ( 'NONE',  ( 31.49298359385885959, -60.71197230342421136, 3.050751728647414840 ) ) ;
#7657 = VERTEX_POINT ( 'NONE', #7993 ) ;
#7658 = AXIS2_PLACEMENT_3D ( 'NONE', #10580, #11563, #9429 ) ;
#7659 = CARTESIAN_POINT ( 'NONE',  ( -8.842479278987921631, -7.118053859731281463, 48.00000000000012079 ) ) ;
#7660 = CARTESIAN_POINT ( 'NONE',  ( -12.41494337171168283, -9.406612424898836977, 57.50000000000012079 ) ) ;
#7661 = CIRCLE ( 'NONE', #10363, 0.7892041907098262810 ) ;
#7662 = CARTESIAN_POINT ( 'NONE',  ( 10.23047706855497196, -60.71197230342421847, 3.050751728647392191 ) ) ;
#7663 = FACE_OUTER_BOUND ( 'NONE', #12595, .T. ) ;
#7664 = CARTESIAN_POINT ( 'NONE',  ( 24.10826840236108737, -69.39711819508849544, 6.201611931792130328 ) ) ;
#7665 = AXIS2_PLACEMENT_3D ( 'NONE', #13168, #6025, #7477 ) ;
#7666 = AXIS2_PLACEMENT_3D ( 'NONE', #12653, #10345, #6961 ) ;
#7667 = CARTESIAN_POINT ( 'NONE',  ( -21.66581936427349575, -2.249290599286303483, 57.50000000000012079 ) ) ;
#7668 = AXIS2_PLACEMENT_3D ( 'NONE', #14426, #13271, #2720 ) ;
#7669 = ORIENTED_EDGE ( 'NONE', *, *, #9322, .T. ) ;
#7670 = FACE_OUTER_BOUND ( 'NONE', #8915, .T. ) ;
#7671 = EDGE_CURVE ( 'NONE', #7044, #8826, #2633, .T. ) ;
#7672 = EDGE_CURVE ( 'NONE', #1762, #13307, #11603, .T. ) ;
#7673 = ORIENTED_EDGE ( 'NONE', *, *, #10360, .F. ) ;
#7674 = LINE ( 'NONE', #5065, #4949 ) ;
#7675 = EDGE_LOOP ( 'NONE', ( #224, #12363, #13230, #10189, #4725, #12188, #13134, #11763, #6957, #12084, #12574, #3681, #7207, #4164, #14006, #13960, #1758, #14741, #98, #11796, #12384, #9778, #9830, #5306 ) ) ;
#7676 = CARTESIAN_POINT ( 'NONE',  ( 56.59738969056744651, 0.000000000000000000, -33.00000000000012790 ) ) ;
#7677 = CARTESIAN_POINT ( 'NONE',  ( 10.23047706855496308, -60.71197230342421136, -3.050751728647428607 ) ) ;
#7678 = AXIS2_PLACEMENT_3D ( 'NONE', #14288, #10526, #11748 ) ;
#7679 = DIRECTION ( 'NONE',  ( 0.8586863916854811096, -0.5125013958363124900, 0.000000000000000000 ) ) ;
#7680 = DIRECTION ( 'NONE',  ( 0.8746197071345572782, -0.4848096202550659650, -0.000000000000000000 ) ) ;
#7681 = ORIENTED_EDGE ( 'NONE', *, *, #11876, .T. ) ;
#7682 = VECTOR ( 'NONE', #9367, 1000.000000000000000 ) ;
#7683 = AXIS2_PLACEMENT_3D ( 'NONE', #14481, #1696, #13538 ) ;
#7684 = CARTESIAN_POINT ( 'NONE',  ( 31.72322230991231962, -61.42570632716525125, -2.132522520905367536 ) ) ;
#7685 = ORIENTED_EDGE ( 'NONE', *, *, #3022, .T. ) ;
#7686 = AXIS2_PLACEMENT_3D ( 'NONE', #5318, #10016, #13546 ) ;
#7687 = CARTESIAN_POINT ( 'NONE',  ( 12.36791015745245836, -52.24929059928630437, -3.199931146564425788 ) ) ;
#7688 = CARTESIAN_POINT ( 'NONE',  ( 52.25109540565180311, -2.012892184189034595, 48.51982618741349285 ) ) ;
#7689 = CARTESIAN_POINT ( 'NONE',  ( 108.0866310645538562, 0.000000000000000000, -33.00000000000012790 ) ) ;
#7690 = EDGE_LOOP ( 'NONE', ( #9118, #14926, #14895, #13440 ) ) ;
#7691 = EDGE_CURVE ( 'NONE', #13591, #13103, #6328, .T. ) ;
#7692 = CARTESIAN_POINT ( 'NONE',  ( 53.04398595309534414, -1.224959495890951100, 48.51982618741349285 ) ) ;
#7693 = ORIENTED_EDGE ( 'NONE', *, *, #13636, .F. ) ;
#7694 = ORIENTED_EDGE ( 'NONE', *, *, #1883, .F. ) ;
#7695 = AXIS2_PLACEMENT_3D ( 'NONE', #5846, #10682, #973 ) ;
#7696 = ORIENTED_EDGE ( 'NONE', *, *, #4673, .F. ) ;
#7697 = AXIS2_PLACEMENT_3D ( 'NONE', #1903, #14681, #9931 ) ;
#7698 = CARTESIAN_POINT ( 'NONE',  ( 62.67308791069655882, 29.52935533987996664, -33.00000000000013500 ) ) ;
#7699 = DIRECTION ( 'NONE',  ( -1.000000000000000000, 0.000000000000000000, 0.000000000000000000 ) ) ;
#7700 = CARTESIAN_POINT ( 'NONE',  ( 112.9262740340969060, 0.000000000000000000, 13.14990448602693007 ) ) ;
#7701 = DIRECTION ( 'NONE',  ( -0.000000000000000000, -0.000000000000000000, 1.000000000000000000 ) ) ;
#7702 = ORIENTED_EDGE ( 'NONE', *, *, #2367, .T. ) ;
#7703 = ORIENTED_EDGE ( 'NONE', *, *, #5794, .T. ) ;
#7704 = CARTESIAN_POINT ( 'NONE',  ( -8.537170960192302260, 2.067018546614596719, -48.00000000000012079 ) ) ;
#7705 = CIRCLE ( 'NONE', #6252, 9.999999999999994671 ) ;
#7706 = CARTESIAN_POINT ( 'NONE',  ( 66.38598137497019991, -11.47113225237461087, 72.19766410831374515 ) ) ;
#7707 = CARTESIAN_POINT ( 'NONE',  ( 69.32504094576864873, -4.037435678230563596, 77.18389507655805915 ) ) ;
#7708 = CIRCLE ( 'NONE', #13602, 3.999999999999999112 ) ;
#7709 = CARTESIAN_POINT ( 'NONE',  ( 105.5545870572953930, -1.749290599286305259, -13.14990448602692474 ) ) ;
#7710 = DIRECTION ( 'NONE',  ( 0.000000000000000000, -0.000000000000000000, -1.000000000000000000 ) ) ;
#7711 = ORIENTED_EDGE ( 'NONE', *, *, #30, .F. ) ;
#7712 = CARTESIAN_POINT ( 'NONE',  ( 32.98163981592925609, -56.83281747056103939, 2.758293468456500808 ) ) ;
#7713 = CARTESIAN_POINT ( 'NONE',  ( -9.198099345814858552, 2.262399347264687943, 48.43121057161710041 ) ) ;
#7714 = ADVANCED_FACE ( 'NONE', ( #14455 ), #7144, .T. ) ;
#7715 = ORIENTED_EDGE ( 'NONE', *, *, #8363, .F. ) ;
#7716 = DIRECTION ( 'NONE',  ( -0.000000000000000000, -0.000000000000000000, 1.000000000000000000 ) ) ;
#7717 = PRESENTATION_STYLE_ASSIGNMENT (( #2007 ) ) ;
#7718 =( NAMED_UNIT ( * ) SI_UNIT ( $, .STERADIAN. ) SOLID_ANGLE_UNIT ( ) );
#7719 = DIRECTION ( 'NONE',  ( -0.8746197071345576113, 0.4848096202550652989, 0.000000000000000000 ) ) ;
#7720 = VERTEX_POINT ( 'NONE', #4913 ) ;
#7721 = EDGE_CURVE ( 'NONE', #3968, #5929, #8529, .T. ) ;
#7722 = DIRECTION ( 'NONE',  ( 0.000000000000000000, 0.000000000000000000, 1.000000000000000000 ) ) ;
#7723 = EDGE_CURVE ( 'NONE', #3752, #4049, #10738, .T. ) ;
#7724 = DIRECTION ( 'NONE',  ( 0.4848096202550659650, 0.8746197071345572782, 0.000000000000000000 ) ) ;
#7725 = FACE_BOUND ( 'NONE', #8032, .T. ) ;
#7726 = EDGE_CURVE ( 'NONE', #1886, #9351, #3455, .T. ) ;
#7727 = CARTESIAN_POINT ( 'NONE',  ( 31.13618595441765180, -61.88944072237682548, -2.366779157396530664 ) ) ;
#7728 = ORIENTED_EDGE ( 'NONE', *, *, #30, .T. ) ;
#7729 = DIRECTION ( 'NONE',  ( -1.000000000000000000, 0.000000000000000000, 0.000000000000000000 ) ) ;
#7730 = EDGE_LOOP ( 'NONE', ( #6992, #8224, #3550, #7502 ) ) ;
#7731 = DIRECTION ( 'NONE',  ( 0.000000000000000000, 0.000000000000000000, 1.000000000000000000 ) ) ;
#7732 = DIRECTION ( 'NONE',  ( 0.000000000000000000, 0.000000000000000000, 1.000000000000000000 ) ) ;
#7733 = ADVANCED_FACE ( 'NONE', ( #8597 ), #75, .T. ) ;
#7734 = ORIENTED_EDGE ( 'NONE', *, *, #4, .T. ) ;
#7735 = FACE_OUTER_BOUND ( 'NONE', #5434, .T. ) ;
#7736 = FACE_OUTER_BOUND ( 'NONE', #7505, .T. ) ;
#7737 = EDGE_CURVE ( 'NONE', #13187, #10116, #14431, .T. ) ;
#7738 = CARTESIAN_POINT ( 'NONE',  ( 13.00536048170750725, -65.29678988936913697, 3.348867343496716220 ) ) ;
#7739 = CARTESIAN_POINT ( 'NONE',  ( 10.55836631292224048, -52.62744651407950869, 3.653242136006523921 ) ) ;
#7740 = CARTESIAN_POINT ( 'NONE',  ( 31.47081793403788552, -52.80574453025635506, -2.610796954002106762 ) ) ;
#7741 = EDGE_CURVE ( 'NONE', #5990, #3172, #7453, .T. ) ;
#7742 = LINE ( 'NONE', #13739, #344 ) ;
#7743 = CARTESIAN_POINT ( 'NONE',  ( 98.40734512546775647, 0.000000000000000000, -33.00000000000012790 ) ) ;
#7744 = VERTEX_POINT ( 'NONE', #4767 ) ;
#7745 = DIRECTION ( 'NONE',  ( 0.000000000000000000, 0.000000000000000000, 1.000000000000000000 ) ) ;
#7746 = ORIENTED_EDGE ( 'NONE', *, *, #1941, .F. ) ;
#7747 =( BOUNDED_SURFACE ( )  B_SPLINE_SURFACE ( 3, 2, ( 
 ( #12614, #12855, #13843 ),
 ( #1063, #13441, #9386 ),
 ( #6754, #2302, #11760 ),
 ( #10458, #5617, #3219 ) ),
 .UNSPECIFIED., .F., .F., .F. ) 
 B_SPLINE_SURFACE_WITH_KNOTS ( ( 4, 4 ),
 ( 3, 3 ),
 ( -6.071532165918824830E-18, 0.001771943201165730774 ),
 ( 0.000000000000000000, 1.000000000000000000 ),
 .UNSPECIFIED. ) 
 GEOMETRIC_REPRESENTATION_ITEM ( )  RATIONAL_B_SPLINE_SURFACE ( (
 ( 1.000000000000000000, 0.8308543624379416404, 1.000000000000000000),
 ( 1.000000000000000000, 0.8288551047899437307, 1.000000000000000000),
 ( 1.000000000000000000, 0.8269348987755770208, 1.000000000000000000),
 ( 1.000000000000000000, 0.8250833044923663318, 1.000000000000000000) ) ) 
 REPRESENTATION_ITEM ( '' )  SURFACE ( )  );
#7748 = CARTESIAN_POINT ( 'NONE',  ( 30.86690024639267804, -53.50334687180571080, -3.717581709362814291 ) ) ;
#7749 = ORIENTED_EDGE ( 'NONE', *, *, #11660, .F. ) ;
#7750 = DIRECTION ( 'NONE',  ( -0.8420378618367644341, -0.5394184268574535590, 0.000000000000000000 ) ) ;
#7751 = CARTESIAN_POINT ( 'NONE',  ( 60.34603303165619792, -7.282908750500069139, 60.61639468829817190 ) ) ;
#7752 = EDGE_CURVE ( 'NONE', #9584, #3003, #11722, .T. ) ;
#7753 = FACE_OUTER_BOUND ( 'NONE', #10917, .T. ) ;
#7754 = CARTESIAN_POINT ( 'NONE',  ( 54.85055839958032209, 21.75070940071329417, 33.00000000000012790 ) ) ;
#7755 = ORIENTED_EDGE ( 'NONE', *, *, #4092, .F. ) ;
#7756 = DIRECTION ( 'NONE',  ( -1.000000000000000000, 0.000000000000000000, 0.000000000000000000 ) ) ;
#7757 = VERTEX_POINT ( 'NONE', #8311 ) ;
#7758 = EDGE_CURVE ( 'NONE', #1679, #10618, #2452, .T. ) ;
#7759 = EDGE_CURVE ( 'NONE', #3759, #14513, #6005, .T. ) ;
#7760 = DIRECTION ( 'NONE',  ( 0.5006040828730242698, -0.8656763553493062036, 0.000000000000000000 ) ) ;
#7761 = CARTESIAN_POINT ( 'NONE',  ( -25.04138923958014473, -6.321889167469157300, -58.00000000000012079 ) ) ;
#7762 = FACE_OUTER_BOUND ( 'NONE', #6384, .T. ) ;
#7763 = CARTESIAN_POINT ( 'NONE',  ( 84.72310019870096198, 25.52935533987996664, -33.00000000000013500 ) ) ;
#7764 = ORIENTED_EDGE ( 'NONE', *, *, #5724, .T. ) ;
#7765 = TOROIDAL_SURFACE ( 'NONE', #1374, 12.46463184759105047, 1.000000000000000000 ) ;
#7766 = CARTESIAN_POINT ( 'NONE',  ( 40.33162949095117966, 23.25070940071368852, 139.1143251403882459 ) ) ;
#7767 = VERTEX_POINT ( 'NONE', #10688 ) ;
#7768 = CARTESIAN_POINT ( 'NONE',  ( 71.15942379059755751, -15.26044865788734484, 73.19766410831374515 ) ) ;
#7769 = ORIENTED_EDGE ( 'NONE', *, *, #7741, .T. ) ;
#7770 = ORIENTED_EDGE ( 'NONE', *, *, #6065, .F. ) ;
#7771 = DIRECTION ( 'NONE',  ( -0.5394184268574520047, 0.8420378618367654333, 0.000000000000000000 ) ) ;
#7772 = CARTESIAN_POINT ( 'NONE',  ( -8.537170960192302260, 2.067018546614596719, 48.00000000000012079 ) ) ;
#7773 = FACE_OUTER_BOUND ( 'NONE', #9683, .T. ) ;
#7774 = EDGE_CURVE ( 'NONE', #65, #1549, #9618, .T. ) ;
#7775 = CARTESIAN_POINT ( 'NONE',  ( 9.213596949546614567, -54.90226484923774564, -3.064913166935410604 ) ) ;
#7776 = EDGE_CURVE ( 'NONE', #1527, #9198, #13148, .T. ) ;
#7777 = EDGE_LOOP ( 'NONE', ( #865, #4800, #3052, #9549 ) ) ;
#7778 = CARTESIAN_POINT ( 'NONE',  ( 65.00000000000001421, -85.24929059928631148, 19.99999999999999645 ) ) ;
#7779 = CARTESIAN_POINT ( 'NONE',  ( 65.51035252688646437, -10.91538014501780651, 72.13738083359044140 ) ) ;
#7780 = DIRECTION ( 'NONE',  ( 0.000000000000000000, 0.000000000000000000, 1.000000000000000000 ) ) ;
#7781 = CARTESIAN_POINT ( 'NONE',  ( -9.456839514482961562, 2.659958822950721835, 48.50000000000012079 ) ) ;
#7782 = CARTESIAN_POINT ( 'NONE',  ( 63.03271294676726910, -4.597264848142483373, 48.51982618741349285 ) ) ;
#7783 = ORIENTED_EDGE ( 'NONE', *, *, #8348, .F. ) ;
#7784 = CARTESIAN_POINT ( 'NONE',  ( 69.46451092899815194, -2.309308060028171017, 72.92418198763061810 ) ) ;
#7785 = CIRCLE ( 'NONE', #3111, 3.694885682587998765 ) ;
#7786 = VECTOR ( 'NONE', #1588, 1000.000000000000000 ) ;
#7787 = DIRECTION ( 'NONE',  ( -0.000000000000000000, -0.000000000000000000, -1.000000000000000000 ) ) ;
#7788 = ORIENTED_EDGE ( 'NONE', *, *, #14583, .T. ) ;
#7789 = DIRECTION ( 'NONE',  ( 0.000000000000000000, 0.000000000000000000, 1.000000000000000000 ) ) ;
#7790 = CARTESIAN_POINT ( 'NONE',  ( -16.99999999999998579, -6.754727345143736628, 38.00000000000012079 ) ) ;
#7791 = DIRECTION ( 'NONE',  ( -0.8656763553493062036, -0.5006040828730242698, -0.000000000000000000 ) ) ;
#7792 = DIRECTION ( 'NONE',  ( 0.000000000000000000, 1.000000000000000000, -0.000000000000000000 ) ) ;
#7793 = VERTEX_POINT ( 'NONE', #11982 ) ;
#7794 = VECTOR ( 'NONE', #1885, 1000.000000000000000 ) ;
#7795 = AXIS2_PLACEMENT_3D ( 'NONE', #13028, #8412, #1086 ) ;
#7796 = CARTESIAN_POINT ( 'NONE',  ( 8.749224225583514425, -56.32723911702734654, 2.799366360498976913 ) ) ;
#7797 = AXIS2_PLACEMENT_3D ( 'NONE', #5036, #6122, #1494 ) ;
#7798 = CARTESIAN_POINT ( 'NONE',  ( 30.17362133822251735, -53.31455134687480779, 3.969134470563519645 ) ) ;
#7799 = CARTESIAN_POINT ( 'NONE',  ( 63.00747169918385993, -1.516790343742004055, 48.51982618741349285 ) ) ;
#7800 = CARTESIAN_POINT ( 'NONE',  ( -24.83354747574476207, -6.700581361908810152, -48.23896987259369240 ) ) ;
#7801 = VECTOR ( 'NONE', #11892, 1000.000000000000000 ) ;
#7802 = B_SPLINE_CURVE_WITH_KNOTS ( 'NONE', 3,
 ( #5350, #720, #5583, #13656, #4417, #10198, #10280, #4337, #3188, #5425 ),
 .UNSPECIFIED., .F., .F.,
 ( 4, 2, 2, 2, 4 ),
 ( 0.000000000000000000, 0.0006693228878568692692, 0.001338645775713738538, 0.002007968663570607916, 0.002677291551427477077 ),
 .UNSPECIFIED. ) ;
#7803 = VERTEX_POINT ( 'NONE', #2677 ) ;
#7804 = CYLINDRICAL_SURFACE ( 'NONE', #4668, 6.484807146443463566 ) ;
#7805 = ORIENTED_EDGE ( 'NONE', *, *, #9296, .T. ) ;
#7806 = DIRECTION ( 'NONE',  ( 0.000000000000000000, 0.000000000000000000, 1.000000000000000000 ) ) ;
#7807 = DIRECTION ( 'NONE',  ( 1.000000000000000000, -0.000000000000000000, -0.000000000000000000 ) ) ;
#7808 = ADVANCED_FACE ( 'NONE', ( #2823 ), #9842, .F. ) ;
#7809 = VECTOR ( 'NONE', #7791, 1000.000000000000000 ) ;
#7810 = EDGE_LOOP ( 'NONE', ( #11396, #7339, #11607, #825 ) ) ;
#7812 = ORIENTED_EDGE ( 'NONE', *, *, #10897, .T. ) ;
#7811 = DIRECTION ( 'NONE',  ( -0.8656763553493062036, -0.5006040828730242698, -0.000000000000000000 ) ) ;
#7813 = DIRECTION ( 'NONE',  ( -0.000000000000000000, -1.000000000000000000, -0.000000000000000000 ) ) ;
#7814 = EDGE_CURVE ( 'NONE', #9843, #13835, #3971, .T. ) ;
#7815 = ADVANCED_FACE ( 'NONE', ( #12207, #8970 ), #4189, .T. ) ;
#7816 = DIRECTION ( 'NONE',  ( 0.000000000000000000, 0.000000000000000000, 1.000000000000000000 ) ) ;
#7817 = TOROIDAL_SURFACE ( 'NONE', #3143, 8.500000000000000000, 0.5000000000000000000 ) ;
#7818 = CARTESIAN_POINT ( 'NONE',  ( 9.873256694677030154, -53.04884725814041246, 2.499854452449908671 ) ) ;
#7819 = CARTESIAN_POINT ( 'NONE',  ( 32.48670927670975317, -59.22992907132844920, 2.757908842764457802 ) ) ;
#7820 = CARTESIAN_POINT ( 'NONE',  ( -3.190546569013415379, 0.8906624217387615339, 57.50000000000012079 ) ) ;
#7821 = PRODUCT ( 'Plastic-Headed Clamping Screw', 'Plastic-Headed Clamping Screw', '', ( #4064 ) ) ;
#7822 = CARTESIAN_POINT ( 'NONE',  ( 51.75774672102440377, 23.25070940071368852, 33.00000000000012790 ) ) ;
#7823 = CARTESIAN_POINT ( 'NONE',  ( -2.688903428702175252E-15, 23.25070940071368142, -33.00000000000012790 ) ) ;
#7824 = EDGE_CURVE ( 'NONE', #10905, #5061, #12364, .T. ) ;
#7825 = EDGE_LOOP ( 'NONE', ( #3974, #509, #2100, #5314 ) ) ;
#7826 = EDGE_CURVE ( 'NONE', #1838, #4786, #3621, .T. ) ;
#7827 = CARTESIAN_POINT ( 'NONE',  ( 17.53865101128009130, -70.79589105110508740, -6.161139702149304398 ) ) ;
#7828 = EDGE_LOOP ( 'NONE', ( #3994, #10288, #1761, #12700 ) ) ;
#7829 = DIRECTION ( 'NONE',  ( 1.000000000000000000, -6.938893903907228378E-17, 0.000000000000000000 ) ) ;
#7830 = ORIENTED_EDGE ( 'NONE', *, *, #165, .T. ) ;
#7831 = LINE ( 'NONE', #7676, #270 ) ;
#7832 = LINE ( 'NONE', #9986, #8019 ) ;
#7833 = CYLINDRICAL_SURFACE ( 'NONE', #2159, 0.7892041907098261699 ) ;
#7834 = DIRECTION ( 'NONE',  ( -0.000000000000000000, -0.000000000000000000, -1.000000000000000000 ) ) ;
#7835 = PLANE ( 'NONE',  #11089 ) ;
#7836 = ORIENTED_EDGE ( 'NONE', *, *, #2638, .T. ) ;
#7837 = CARTESIAN_POINT ( 'NONE',  ( 65.70654796114106944, -11.75627201178154912, 76.02260248133795528 ) ) ;
#7838 = CARTESIAN_POINT ( 'NONE',  ( 8.102845986945748535, -56.17744385466403401, -1.865378520188700540 ) ) ;
#7839 = CARTESIAN_POINT ( 'NONE',  ( 31.72322230991231962, -61.42570632716525125, 2.500000000000000000 ) ) ;
#7840 = CARTESIAN_POINT ( 'NONE',  ( -10.08688311991301312, -8.022742138608869311, 47.66502101098957667 ) ) ;
#7841 =( BOUNDED_SURFACE ( )  B_SPLINE_SURFACE ( 3, 2, ( 
 ( #6332, #10092, #2937 ),
 ( #14777, #544, #12398 ),
 ( #11307, #8774, #4072 ),
 ( #6477, #1923, #4155 ),
 ( #5397, #3084, #688 ),
 ( #5479, #1847, #4230 ),
 ( #12473, #4008, #13624 ),
 ( #8704, #1777, #5319 ),
 ( #5170, #9949, #11086 ),
 ( #10169, #14851, #4302 ),
 ( #14623, #8933, #13331 ),
 ( #2792, #7485, #13476 ),
 ( #615, #12173, #10017 ),
 ( #1631, #474, #7631 ) ),
 .UNSPECIFIED., .F., .F., .F. ) 
 B_SPLINE_SURFACE_WITH_KNOTS ( ( 4, 2, 2, 2, 2, 2, 4 ),
 ( 3, 3 ),
 ( 0.000000000000000000, 0.002560658414910375533, 0.003840987622365563299, 0.005121316829820751065, 0.006401646037275938832, 0.007681975244731126598, 0.01024263365964150213 ),
 ( 0.000000000000000000, 1.000000000000000000 ),
 .UNSPECIFIED. ) 
 GEOMETRIC_REPRESENTATION_ITEM ( )  RATIONAL_B_SPLINE_SURFACE ( (
 ( 1.000000000000000000, 0.8053615646146053964, 1.000000000000000000),
 ( 1.000000000000000000, 0.8105996499491067153, 1.000000000000000000),
 ( 1.000000000000000000, 0.8160199193853723276, 1.000000000000000000),
 ( 1.000000000000000000, 0.8240376314735106122, 1.000000000000000000),
 ( 1.000000000000000000, 0.8266971106456151297, 1.000000000000000000),
 ( 1.000000000000000000, 0.8319110421176818537, 1.000000000000000000),
 ( 1.000000000000000000, 0.8344214672177640013, 1.000000000000000000),
 ( 1.000000000000000000, 0.8392107060239336613, 1.000000000000000000),
 ( 1.000000000000000000, 0.8414897010532279564, 1.000000000000000000),
 ( 1.000000000000000000, 0.8457750297009817286, 1.000000000000000000),
 ( 1.000000000000000000, 0.8477871175333712150, 1.000000000000000000),
 ( 1.000000000000000000, 0.8533050377660172936, 1.000000000000000000),
 ( 1.000000000000000000, 0.8561733496716913416, 1.000000000000000000),
 ( 1.000000000000000000, 0.8581891718822912685, 1.000000000000000000) ) ) 
 REPRESENTATION_ITEM ( '' )  SURFACE ( )  );
#7842 = ORIENTED_EDGE ( 'NONE', *, *, #13536, .F. ) ;
#7843 = B_SPLINE_CURVE_WITH_KNOTS ( 'NONE', 3,
 ( #4769, #78, #3536, #8154, #10691, #2534, #4993, #8237, #9463, #2304 ),
 .UNSPECIFIED., .F., .F.,
 ( 4, 2, 2, 2, 4 ),
 ( 0.000000000000000000, 0.0004999547661763326014, 0.0009999095323526652028, 0.001499864298528997804, 0.001999819064705330406 ),
 .UNSPECIFIED. ) ;
#7844 = DIRECTION ( 'NONE',  ( -1.000000000000000000, 0.000000000000000000, 0.000000000000000000 ) ) ;
#7845 = ORIENTED_EDGE ( 'NONE', *, *, #6605, .T. ) ;
#7846 = CARTESIAN_POINT ( 'NONE',  ( 49.07597535787931520, -2.249290599286309256, 47.51982618741348574 ) ) ;
#7847 = ORIENTED_EDGE ( 'NONE', *, *, #8643, .F. ) ;
#7848 = ORIENTED_EDGE ( 'NONE', *, *, #684, .T. ) ;
#7849 = ADVANCED_FACE ( 'NONE', ( #585 ), #2871, .T. ) ;
#7850 = SURFACE_STYLE_FILL_AREA ( #6528 ) ;
#7851 = CARTESIAN_POINT ( 'NONE',  ( 9.359011486233180577, -60.82759157437174480, -1.965556376683131212 ) ) ;
#7852 = CARTESIAN_POINT ( 'NONE',  ( -22.46208338003149407, 4.939996070762163960, -48.38299871081639481 ) ) ;
#7853 = AXIS2_PLACEMENT_3D ( 'NONE', #13328, #12102, #6189 ) ;
#7854 = AXIS2_PLACEMENT_3D ( 'NONE', #3096, #4170, #8868 ) ;
#7855 = LINE ( 'NONE', #2073, #6297 ) ;
#7856 = CARTESIAN_POINT ( 'NONE',  ( 73.69809405469877106, 25.52935533987996664, -27.49288055531513209 ) ) ;
#7857 = ORIENTED_EDGE ( 'NONE', *, *, #8846, .F. ) ;
#7858 = CARTESIAN_POINT ( 'NONE',  ( 27.86173033120691045, -69.39711819508849544, 3.619682905202613377 ) ) ;
#7859 = DIRECTION ( 'NONE',  ( 0.000000000000000000, -0.000000000000000000, 1.000000000000000000 ) ) ;
#7860 = PLANE ( 'NONE',  #5638 ) ;
#7861 = CARTESIAN_POINT ( 'NONE',  ( 19.97461805067967688, -85.24929059928631148, -6.000000000000000888 ) ) ;
#7862 = CYLINDRICAL_SURFACE ( 'NONE', #4666, 4.000000000000003553 ) ;
#7863 = VERTEX_POINT ( 'NONE', #13367 ) ;
#7864 = CARTESIAN_POINT ( 'NONE',  ( 32.96722027535705735, -56.32851134755744482, 2.801743212233187563 ) ) ;
#7865 = CIRCLE ( 'NONE', #5663, 3.694885682587998765 ) ;
#7866 = DIRECTION ( 'NONE',  ( 1.000000000000000000, 0.000000000000000000, 0.000000000000000000 ) ) ;
#7867 = VERTEX_POINT ( 'NONE', #507 ) ;
#7868 = ADVANCED_FACE ( 'NONE', ( #9979 ), #5209, .F. ) ;
#7869 = PLANE ( 'NONE',  #11271 ) ;
#7870 = CARTESIAN_POINT ( 'NONE',  ( -3.285520523749251520, 5.681530634151883419, -48.50000000000012079 ) ) ;
#7871 = DIRECTION ( 'NONE',  ( 0.000000000000000000, -1.000000000000000000, 0.000000000000000000 ) ) ;
#7872 = LINE ( 'NONE', #12564, #7523 ) ;
#7873 = VECTOR ( 'NONE', #7787, 1000.000000000000000 ) ;
#7874 = DIRECTION ( 'NONE',  ( 1.000000000000000000, 0.000000000000000000, -0.000000000000000000 ) ) ;
#7875 = DIRECTION ( 'NONE',  ( -0.000000000000000000, -0.000000000000000000, 1.000000000000000000 ) ) ;
#7876 = CARTESIAN_POINT ( 'NONE',  ( 67.21328690825531282, 22.43695620243006772, -33.00000000000012790 ) ) ;
#7877 = DIRECTION ( 'NONE',  ( -1.000000000000000000, -2.775557561562891351E-15, 0.000000000000000000 ) ) ;
#7878 = ORIENTED_EDGE ( 'NONE', *, *, #1031, .T. ) ;
#7879 = ORIENTED_EDGE ( 'NONE', *, *, #5199, .F. ) ;
#7880 = EDGE_CURVE ( 'NONE', #13865, #4611, #1877, .T. ) ;
#7881 = CARTESIAN_POINT ( 'NONE',  ( 24.31690506110717465, -73.00063092935944553, -6.088059227065252266 ) ) ;
#7882 = VERTEX_POINT ( 'NONE', #8735 ) ;
#7883 = LINE ( 'NONE', #12577, #1751 ) ;
#7884 = CARTESIAN_POINT ( 'NONE',  ( 65.00000000000001421, -85.24929059928631148, 22.52499999999999503 ) ) ;
#7885 = ORIENTED_EDGE ( 'NONE', *, *, #3435, .T. ) ;
#7886 = DIRECTION ( 'NONE',  ( 0.000000000000000000, 1.000000000000000000, -0.000000000000000000 ) ) ;
#7887 = FACE_OUTER_BOUND ( 'NONE', #11849, .T. ) ;
#7888 = CARTESIAN_POINT ( 'NONE',  ( 13.13160920566097367, -64.18054652438900121, 4.118450070759805293 ) ) ;
#7889 = AXIS2_PLACEMENT_3D ( 'NONE', #3578, #6128, #7347 ) ;
#7890 = ADVANCED_FACE ( 'NONE', ( #7670 ), #13150, .T. ) ;
#7891 = DIRECTION ( 'NONE',  ( 0.000000000000000000, -0.000000000000000000, -1.000000000000000000 ) ) ;
#7892 = CARTESIAN_POINT ( 'NONE',  ( 54.00000000000000711, -2.249290599286311032, -33.00000000000012790 ) ) ;
#7893 = LINE ( 'NONE', #12588, #8862 ) ;
#7894 = FACE_OUTER_BOUND ( 'NONE', #7675, .T. ) ;
#7895 = CARTESIAN_POINT ( 'NONE',  ( 118.0000000000000284, 19.25070940071370273, 139.1143251403882459 ) ) ;
#7896 = ORIENTED_EDGE ( 'NONE', *, *, #14591, .T. ) ;
#7897 = CARTESIAN_POINT ( 'NONE',  ( 7.982950795113611164, -53.52517728513006290, -2.732533236877404903 ) ) ;
#7898 = AXIS2_PLACEMENT_3D ( 'NONE', #2261, #8353, #9586 ) ;
#7899 = EDGE_LOOP ( 'NONE', ( #13644, #10077, #6002, #13497 ) ) ;
#7900 = CARTESIAN_POINT ( 'NONE',  ( 32.94092596975102083, -56.07151166541879661, -2.830535587930123942 ) ) ;
#7901 = CIRCLE ( 'NONE', #9138, 4.000000000000003553 ) ;
#7902 = ORIENTED_EDGE ( 'NONE', *, *, #6998, .F. ) ;
#7903 = CARTESIAN_POINT ( 'NONE',  ( -2.016677571526633510E-15, 23.25070940071368497, 33.00000000000012790 ) ) ;
#7904 = EDGE_CURVE ( 'NONE', #9598, #3404, #3123, .T. ) ;
#7905 = DIRECTION ( 'NONE',  ( -0.8746197071345572782, 0.4848096202550660205, 0.000000000000000000 ) ) ;
#7906 = B_SPLINE_CURVE_WITH_KNOTS ( 'NONE', 3,
 ( #6971, #12752, #11658, #7042, #14973, #11738, #8285, #12981, #9359, #6889 ),
 .UNSPECIFIED., .F., .F.,
 ( 4, 2, 2, 2, 4 ),
 ( 0.000000000000000000, 0.0004995983118107942761, 0.0009991966236215885522, 0.001498794935432382937, 0.001998393247243177104 ),
 .UNSPECIFIED. ) ;
#7907 = FACE_OUTER_BOUND ( 'NONE', #9721, .T. ) ;
#7908 = CARTESIAN_POINT ( 'NONE',  ( 33.52235686305655804, -57.48563641131178770, -1.816685854991392457 ) ) ;
#7909 = EDGE_CURVE ( 'NONE', #14799, #8767, #2390, .T. ) ;
#7910 = EDGE_CURVE ( 'NONE', #14077, #15028, #4852, .T. ) ;
#7911 = CYLINDRICAL_SURFACE ( 'NONE', #293, 5.496540510819668768 ) ;
#7912 = EDGE_CURVE ( 'NONE', #14241, #4729, #8130, .T. ) ;
#7913 = VECTOR ( 'NONE', #8254, 1000.000000000000000 ) ;
#7914 = ORIENTED_EDGE ( 'NONE', *, *, #2779, .T. ) ;
#7915 = VECTOR ( 'NONE', #10215, 1000.000000000000000 ) ;
#7916 = VECTOR ( 'NONE', #3725, 1000.000000000000114 ) ;
#7917 = DIRECTION ( 'NONE',  ( -0.000000000000000000, -0.000000000000000000, -1.000000000000000000 ) ) ;
#7918 = CARTESIAN_POINT ( 'NONE',  ( 8.760785244683058082, -54.21582538152134134, -2.947777686198771452 ) ) ;
#7919 = DIRECTION ( 'NONE',  ( -1.000000000000000000, 0.000000000000000000, 0.000000000000000000 ) ) ;
#7920 = CARTESIAN_POINT ( 'NONE',  ( 70.46453521882889959, -2.298370886119723622, 75.19766410831374515 ) ) ;
#7921 = EDGE_CURVE ( 'NONE', #2105, #7961, #10499, .T. ) ;
#7922 = ORIENTED_EDGE ( 'NONE', *, *, #10733, .T. ) ;
#7923 = DIRECTION ( 'NONE',  ( -0.5006040828730989878, 0.8656763553492631269, 0.000000000000000000 ) ) ;
#7924 = ORIENTED_EDGE ( 'NONE', *, *, #6045, .F. ) ;
#7925 = DIRECTION ( 'NONE',  ( 0.5125013958363011657, 0.8586863916854879930, -0.000000000000000000 ) ) ;
#7926 = ORIENTED_EDGE ( 'NONE', *, *, #7632, .F. ) ;
#7927 = VECTOR ( 'NONE', #1470, 999.9999999999998863 ) ;
#7928 = VECTOR ( 'NONE', #12690, 1000.000000000000000 ) ;
#7929 = PLANE ( 'NONE',  #8028 ) ;
#7930 = CARTESIAN_POINT ( 'NONE',  ( 20.86173033120691045, -72.24929059928631148, 0.000000000000000000 ) ) ;
#7931 = AXIS2_PLACEMENT_3D ( 'NONE', #5782, #10696, #3541 ) ;
#7932 = DIRECTION ( 'NONE',  ( -0.000000000000000000, 0.000000000000000000, 1.000000000000000000 ) ) ;
#7933 = CARTESIAN_POINT ( 'NONE',  ( 33.52235686305655804, -57.48563641131178770, 1.816685854991380911 ) ) ;
#7934 = VERTEX_POINT ( 'NONE', #14891 ) ;
#7935 = DIRECTION ( 'NONE',  ( -1.000000000000000000, 0.000000000000000000, 0.000000000000000000 ) ) ;
#7936 = CARTESIAN_POINT ( 'NONE',  ( 69.46189398880601118, -2.505105728916043883, 76.08256302136429383 ) ) ;
#7937 = DIRECTION ( 'NONE',  ( 0.6198786537240922323, 0.7846976836063727090, 0.000000000000000000 ) ) ;
#7938 = CARTESIAN_POINT ( 'NONE',  ( 27.98508387849643242, -66.12497772677620844, 4.110792498118536642 ) ) ;
#7939 = EDGE_LOOP ( 'NONE', ( #6975, #5742, #9609, #2491 ) ) ;
#7940 = VECTOR ( 'NONE', #1520, 1000.000000000000000 ) ;
#7941 = CARTESIAN_POINT ( 'NONE',  ( 46.91810375148135392, 21.75070940071322667, -33.00000000000012790 ) ) ;
#7942 = CIRCLE ( 'NONE', #7450, 4.000000000000003553 ) ;
#7943 = CARTESIAN_POINT ( 'NONE',  ( 33.12442989620986822, -59.21224831720011395, -1.832439066039627251 ) ) ;
#7944 = VERTEX_POINT ( 'NONE', #5827 ) ;
#7945 = CARTESIAN_POINT ( 'NONE',  ( 0.000000000000000000, 21.75070940071325865, 33.00000000000012790 ) ) ;
#7946 = DIRECTION ( 'NONE',  ( 0.000000000000000000, 1.000000000000000000, 0.000000000000000000 ) ) ;
#7947 = EDGE_LOOP ( 'NONE', ( #3405, #13130, #2734, #1719 ) ) ;
#7948 = CARTESIAN_POINT ( 'NONE',  ( 57.92627403409715470, 23.25070940071368852, 33.00000000000012790 ) ) ;
#7949 = DIRECTION ( 'NONE',  ( -0.5454721580263366398, 0.8381289428352246551, 4.385647630081457888E-16 ) ) ;
#7950 = ORIENTED_EDGE ( 'NONE', *, *, #8077, .T. ) ;
#7951 = CARTESIAN_POINT ( 'NONE',  ( 88.00000000000001421, 10.75070940071369208, 33.00000000000014211 ) ) ;
#7952 = AXIS2_PLACEMENT_3D ( 'NONE', #13000, #9456, #12768 ) ;
#7953 = VECTOR ( 'NONE', #5943, 1000.000000000000000 ) ;
#7954 = ADVANCED_FACE ( 'NONE', ( #7978 ), #960, .F. ) ;
#7955 = LINE ( 'NONE', #3329, #13718 ) ;
#7956 = LINE ( 'NONE', #935, #1937 ) ;
#7957 = ADVANCED_FACE ( 'NONE', ( #6814 ), #2548, .F. ) ;
#7958 = CARTESIAN_POINT ( 'NONE',  ( 55.17185982823698964, 2.720345114498381456, 48.51982618741349285 ) ) ;
#7959 = CARTESIAN_POINT ( 'NONE',  ( 32.90197589884652274, -57.33450387999030795, 2.749014434309885235 ) ) ;
#7960 = ORIENTED_EDGE ( 'NONE', *, *, #14118, .T. ) ;
#7961 = VERTEX_POINT ( 'NONE', #6736 ) ;
#7962 = CARTESIAN_POINT ( 'NONE',  ( 32.45057671215001704, -59.39518542680177404, 2.758694842812651871 ) ) ;
#7963 = ORIENTED_EDGE ( 'NONE', *, *, #9015, .F. ) ;
#7964 = CARTESIAN_POINT ( 'NONE',  ( 96.00000000000002842, 2.750709400713692965, -33.00000000000012790 ) ) ;
#7965 = AXIS2_PLACEMENT_3D ( 'NONE', #10063, #14747, #3288 ) ;
#7966 = VERTEX_POINT ( 'NONE', #2202 ) ;
#7967 = CARTESIAN_POINT ( 'NONE',  ( 53.04398595309534414, -1.224959495890951100, 60.61639468829817190 ) ) ;
#7968 = CARTESIAN_POINT ( 'NONE',  ( 103.2469880950108063, 0.000000000000000000, 139.1143251403882459 ) ) ;
#7969 = DIRECTION ( 'NONE',  ( -0.000000000000000000, -0.000000000000000000, -1.000000000000000000 ) ) ;
#7970 = EDGE_CURVE ( 'NONE', #2219, #11665, #11419, .T. ) ;
#7971 = EDGE_CURVE ( 'NONE', #1691, #13383, #3434, .T. ) ;
#7972 = LINE ( 'NONE', #13736, #5341 ) ;
#7973 = CARTESIAN_POINT ( 'NONE',  ( 30.60506088226031096, -52.42380682680348514, -2.856405385968803667 ) ) ;
#7974 = CARTESIAN_POINT ( 'NONE',  ( -16.99999999999998579, -2.249290599286303927, 38.00000000000012079 ) ) ;
#7975 = CARTESIAN_POINT ( 'NONE',  ( 69.97972559857382180, -3.172990593254279457, 75.19766410831374515 ) ) ;
#7976 = CARTESIAN_POINT ( 'NONE',  ( -16.99999999999998579, -2.249290599286303927, -48.00000000000012079 ) ) ;
#7977 = ORIENTED_EDGE ( 'NONE', *, *, #3799, .T. ) ;
#7978 = FACE_OUTER_BOUND ( 'NONE', #8473, .T. ) ;
#7979 = EDGE_LOOP ( 'NONE', ( #10990, #4849 ) ) ;
#7980 = CARTESIAN_POINT ( 'NONE',  ( 32.97423643683031003, -56.32723911702735364, -2.799366360498969364 ) ) ;
#7981 = ORIENTED_EDGE ( 'NONE', *, *, #8104, .T. ) ;
#7982 = DIRECTION ( 'NONE',  ( 0.7398406760702320728, 0.6727821148276328378, 0.000000000000000000 ) ) ;
#7983 = FACE_OUTER_BOUND ( 'NONE', #9737, .T. ) ;
#7984 = FACE_OUTER_BOUND ( 'NONE', #1370, .T. ) ;
#7985 = DIRECTION ( 'NONE',  ( -1.000000000000000000, 0.000000000000000000, 0.000000000000000000 ) ) ;
#7986 = DIRECTION ( 'NONE',  ( -0.8746197071345570562, 0.4848096202550662981, 0.000000000000000000 ) ) ;
#7987 = ORIENTED_EDGE ( 'NONE', *, *, #9818, .F. ) ;
#7988 = CARTESIAN_POINT ( 'NONE',  ( 9.211295467215947497, 29.36814620404575038, 75.19766410831374515 ) ) ;
#7989 = CARTESIAN_POINT ( 'NONE',  ( 8.747270541876149608, -56.45473609427328654, -2.788978005137394689 ) ) ;
#7990 = DIRECTION ( 'NONE',  ( 0.000000000000000000, 0.000000000000000000, -1.000000000000000000 ) ) ;
#7991 = EDGE_CURVE ( 'NONE', #6024, #11520, #2128, .T. ) ;
#7992 = ORIENTED_EDGE ( 'NONE', *, *, #11873, .T. ) ;
#7993 = CARTESIAN_POINT ( 'NONE',  ( -28.95977857253358323, -8.587818791446787614, 48.00000000000012079 ) ) ;
#7994 = VERTEX_POINT ( 'NONE', #14366 ) ;
#7995 = CARTESIAN_POINT ( 'NONE',  ( 53.41380296247595538, -0.1096349785133995947, 48.51982618741349285 ) ) ;
#7996 = ORIENTED_EDGE ( 'NONE', *, *, #7653, .F. ) ;
#7997 = CARTESIAN_POINT ( 'NONE',  ( 10.00023835250034843, -61.42570632716434176, -2.132522520905085539 ) ) ;
#7998 = DIRECTION ( 'NONE',  ( 0.000000000000000000, 1.000000000000000000, -0.000000000000000000 ) ) ;
#7999 = EDGE_CURVE ( 'NONE', #7249, #1762, #12986, .T. ) ;
#8000 = ADVANCED_FACE ( 'NONE', ( #2434 ), #7202, .F. ) ;
#8001 = DIRECTION ( 'NONE',  ( 0.000000000000000000, -0.000000000000000000, 1.000000000000000000 ) ) ;
#8002 = CARTESIAN_POINT ( 'NONE',  ( 118.0000000000000284, 19.25070940071370273, -13.14990448602693007 ) ) ;
#8003 = ORIENTED_EDGE ( 'NONE', *, *, #13272, .T. ) ;
#8004 = VECTOR ( 'NONE', #7701, 1000.000000000000000 ) ;
#8005 = DIRECTION ( 'NONE',  ( -1.000000000000000000, -1.156482317317870492E-16, 0.000000000000000000 ) ) ;
#8006 = LINE ( 'NONE', #11533, #9635 ) ;
#8007 = CARTESIAN_POINT ( 'NONE',  ( 32.95681302906984911, -57.08478275174050509, -2.747861298826744125 ) ) ;
#8008 = CARTESIAN_POINT ( 'NONE',  ( 12.03298173962126150, -53.28399145779480506, -4.141535524925039624 ) ) ;
#8009 = DIRECTION ( 'NONE',  ( -1.000000000000000000, 0.000000000000000000, 0.000000000000000000 ) ) ;
#8010 = ORIENTED_EDGE ( 'NONE', *, *, #6370, .F. ) ;
#8011 = DIRECTION ( 'NONE',  ( 0.4543483311474731945, -0.8908241094534353754, -0.000000000000000000 ) ) ;
#8012 = ADVANCED_FACE ( 'NONE', ( #4817, #13206, #11743 ), #8218, .F. ) ;
#8013 = EDGE_CURVE ( 'NONE', #12681, #11983, #5044, .T. ) ;
#8014 = DIRECTION ( 'NONE',  ( 0.000000000000000000, 0.000000000000000000, 1.000000000000000000 ) ) ;
#8015 = ORIENTED_EDGE ( 'NONE', *, *, #10928, .T. ) ;
#8016 = DIRECTION ( 'NONE',  ( 0.000000000000000000, -0.000000000000000000, 1.000000000000000000 ) ) ;
#8017 = DIRECTION ( 'NONE',  ( -0.2245701561649903200, -0.9744137433416084626, -0.009279102705857585065 ) ) ;
#8018 = ORIENTED_EDGE ( 'NONE', *, *, #1457, .T. ) ;
#8019 = VECTOR ( 'NONE', #733, 1000.000000000000000 ) ;
#8020 = CARTESIAN_POINT ( 'NONE',  ( -9.426221351844976226, -7.120495567270975101, -47.92899112040988996 ) ) ;
#8021 = CARTESIAN_POINT ( 'NONE',  ( 51.75774672102440377, 23.25070940071368852, -33.00000000000012790 ) ) ;
#8022 = ORIENTED_EDGE ( 'NONE', *, *, #10410, .F. ) ;
#8023 = DIRECTION ( 'NONE',  ( -1.000000000000000000, -0.000000000000000000, -0.000000000000000000 ) ) ;
#8024 = DIRECTION ( 'NONE',  ( 1.156482317317870492E-16, -1.000000000000000000, 0.000000000000000000 ) ) ;
#8025 = CARTESIAN_POINT ( 'NONE',  ( 98.40734512546775647, 21.75070940071359615, -33.00000000000012790 ) ) ;
#8026 = CARTESIAN_POINT ( 'NONE',  ( 13.15381962123460191, -65.59433601606471598, 3.409308316089458835 ) ) ;
#8027 = CARTESIAN_POINT ( 'NONE',  ( 25.81270058232203013, 21.75070940071309167, 139.1143251403882459 ) ) ;
#8028 = AXIS2_PLACEMENT_3D ( 'NONE', #12623, #10544, #4920 ) ;
#8029 = FACE_OUTER_BOUND ( 'NONE', #454, .T. ) ;
#8030 = CIRCLE ( 'NONE', #14428, 0.5000000000000001110 ) ;
#8031 = VERTEX_POINT ( 'NONE', #354 ) ;
#8032 = EDGE_LOOP ( 'NONE', ( #11272, #5985, #11759, #12759, #14977, #5197, #4141, #14686, #6606, #6163, #10594, #3299, #5083, #2759, #10945, #13398, #10315, #6813, #6131, #10768, #3437, #6756, #2103, #7702, #7358, #1064, #3074, #5137, #14367, #13846, #8953, #7805, #11816, #14641, #2454 ) ) ;
#8033 = FACE_OUTER_BOUND ( 'NONE', #6069, .T. ) ;
#8034 = AXIS2_PLACEMENT_3D ( 'NONE', #14592, #5435, #6583 ) ;
#8035 = ORIENTED_EDGE ( 'NONE', *, *, #4076, .F. ) ;
#8036 = CARTESIAN_POINT ( 'NONE',  ( 8.149027651920247806, -55.81410829992091749, -1.898795180179252196 ) ) ;
#8037 = CARTESIAN_POINT ( 'NONE',  ( 23.63986771004770659, -58.63441909321034018, 6.426091441073435995 ) ) ;
#8038 = EDGE_LOOP ( 'NONE', ( #14697, #11754, #6491, #3809 ) ) ;
#8039 = CARTESIAN_POINT ( 'NONE',  ( -1.197457146693684082, -2.220571218158921223, 58.00000000000012079 ) ) ;
#8040 = LINE ( 'NONE', #5817, #7293 ) ;
#8041 = EDGE_CURVE ( 'NONE', #12295, #13132, #9521, .T. ) ;
#8042 = AXIS2_PLACEMENT_3D ( 'NONE', #9433, #13191, #4959 ) ;
#8043 = DIRECTION ( 'NONE',  ( 0.000000000000000000, 0.000000000000000000, 1.000000000000000000 ) ) ;
#8044 = EDGE_CURVE ( 'NONE', #2182, #14878, #3585, .T. ) ;
#8045 = FACE_OUTER_BOUND ( 'NONE', #6593, .T. ) ;
#8046 = CARTESIAN_POINT ( 'NONE',  ( 33.32712355835607809, -54.93247203738341966, -2.014559788973314891 ) ) ;
#8047 = AXIS2_PLACEMENT_3D ( 'NONE', #2064, #13840, #3296 ) ;
#8048 = FACE_OUTER_BOUND ( 'NONE', #13300, .T. ) ;
#8049 = CARTESIAN_POINT ( 'NONE',  ( 109.8334623555409735, 21.75070940071366365, -13.14990448602693007 ) ) ;
#8050 = CONICAL_SURFACE ( 'NONE', #7063, 2.524999999999999467, 0.7853981633973787790 ) ;
#8051 = DIRECTION ( 'NONE',  ( 2.042496995908176064E-14, 0.000000000000000000, -1.000000000000000000 ) ) ;
#8052 = EDGE_LOOP ( 'NONE', ( #11381, #89, #7734, #4770 ) ) ;
#8053 = CIRCLE ( 'NONE', #6342, 0.7892041907098259479 ) ;
#8054 = CARTESIAN_POINT ( 'NONE',  ( 8.288157001243341426, -55.00412896302379551, -2.731447707962757931 ) ) ;
#8055 = EDGE_LOOP ( 'NONE', ( #521, #605, #2938, #2698 ) ) ;
#8056 = CARTESIAN_POINT ( 'NONE',  ( 8.127793058700618190, -57.16753985542792549, 1.814554119516831099 ) ) ;
#8057 = ORIENTED_EDGE ( 'NONE', *, *, #6147, .F. ) ;
#8058 =( NAMED_UNIT ( * ) PLANE_ANGLE_UNIT ( ) SI_UNIT ( $, .RADIAN. ) );
#8059 = EDGE_CURVE ( 'NONE', #5398, #10712, #5331, .T. ) ;
#8060 = DIRECTION ( 'NONE',  ( 0.000000000000000000, 0.000000000000000000, 1.000000000000000000 ) ) ;
#8061 = EDGE_CURVE ( 'NONE', #13501, #5867, #13934, .T. ) ;
#8062 = CARTESIAN_POINT ( 'NONE',  ( 23.96426235118329728, -66.70789582472755797, -6.276998965480673931 ) ) ;
#8063 = AXIS2_PLACEMENT_3D ( 'NONE', #13581, #12357, #3963 ) ;
#8064 = AXIS2_PLACEMENT_3D ( 'NONE', #14051, #4742, #10356 ) ;
#8065 = EDGE_LOOP ( 'NONE', ( #4670, #6724, #7770, #6457, #4775, #6302, #14595, #7098, #1306, #959, #5558, #10172, #14319, #4303, #6677, #1590, #8393, #13710, #2777, #8501, #8228, #277, #7749, #4381, #7218, #5969, #12060, #12043, #900, #5006, #8859, #2828, #5085, #4354, #6978 ) ) ;
#8066 = DIRECTION ( 'NONE',  ( -0.000000000000000000, -0.000000000000000000, -1.000000000000000000 ) ) ;
#8067 = CARTESIAN_POINT ( 'NONE',  ( 10.43042538306565881, -53.70781053471295508, -3.558938939092199938 ) ) ;
#8068 = LINE ( 'NONE', #15077, #13110 ) ;
#8069 = CARTESIAN_POINT ( 'NONE',  ( 120.7275739462170918, -41.59316888568430670, 52.68020260152231060 ) ) ;
#8070 = AXIS2_PLACEMENT_3D ( 'NONE', #2160, #8011, #8252 ) ;
#8071 = ORIENTED_EDGE ( 'NONE', *, *, #12312, .F. ) ;
#8072 = DIRECTION ( 'NONE',  ( -0.000000000000000000, -0.000000000000000000, 1.000000000000000000 ) ) ;
#8073 = EDGE_LOOP ( 'NONE', ( #13422, #5439, #3339, #13303 ) ) ;
#8074 = CARTESIAN_POINT ( 'NONE',  ( 76.14589960879430919, -7.734310727912411920, 75.19766410831374515 ) ) ;
#8075 = TOROIDAL_SURFACE ( 'NONE', #2171, 9.500000000000001776, 0.5000000000000000000 ) ;
#8076 = ORIENTED_EDGE ( 'NONE', *, *, #1823, .T. ) ;
#8077 = EDGE_CURVE ( 'NONE', #5759, #6007, #11964, .T. ) ;
#8078 = VERTEX_POINT ( 'NONE', #14213 ) ;
#8079 = DIRECTION ( 'NONE',  ( 0.8746197071345576113, -0.4848096202550652434, 0.000000000000000000 ) ) ;
#8080 = CARTESIAN_POINT ( 'NONE',  ( 40.33162949095117966, 21.75070940071319114, -33.00000000000012790 ) ) ;
#8081 = EDGE_LOOP ( 'NONE', ( #10568, #12350, #12933, #10842, #13039 ) ) ;
#8082 = DIRECTION ( 'NONE',  ( 0.4543483311474630915, -0.8908241094534405935, 0.000000000000000000 ) ) ;
#8083 = LINE ( 'NONE', #11450, #8162 ) ;
#8084 = ORIENTED_EDGE ( 'NONE', *, *, #12441, .F. ) ;
#8085 = DIRECTION ( 'NONE',  ( 1.000000000000000000, 0.000000000000000000, 0.000000000000000000 ) ) ;
#8086 = DIRECTION ( 'NONE',  ( -0.000000000000000000, 1.000000000000000000, 1.445602896647339163E-16 ) ) ;
#8087 = CARTESIAN_POINT ( 'NONE',  ( 27.25618691384012138, -52.24929059928630437, 3.946674197029100384 ) ) ;
#8088 = CARTESIAN_POINT ( 'NONE',  ( 24.01697609496477526, -67.68160391986639013, 6.249260988556712526 ) ) ;
#8089 = ORIENTED_EDGE ( 'NONE', *, *, #1721, .F. ) ;
#8090 = CARTESIAN_POINT ( 'NONE',  ( 69.37724578219226146, -3.713350840992164947, 72.17980951935048495 ) ) ;
#8091 = EDGE_CURVE ( 'NONE', #12939, #9315, #416, .T. ) ;
#8092 = ORIENTED_EDGE ( 'NONE', *, *, #12424, .T. ) ;
#8093 = DIRECTION ( 'NONE',  ( -0.000000000000000000, 0.000000000000000000, -1.000000000000000000 ) ) ;
#8094 = AXIS2_PLACEMENT_3D ( 'NONE', #4088, #7568, #13487 ) ;
#8095 = DIRECTION ( 'NONE',  ( 1.000000000000000000, 0.000000000000000000, 0.000000000000000000 ) ) ;
#8096 = AXIS2_PLACEMENT_3D ( 'NONE', #2094, #2413, #6954 ) ;
#8097 = EDGE_LOOP ( 'NONE', ( #5275, #8739, #11618, #10726 ) ) ;
#8098 = DIRECTION ( 'NONE',  ( 0.000000000000000000, 0.000000000000000000, -1.000000000000000000 ) ) ;
#8099 = CARTESIAN_POINT ( 'NONE',  ( -9.855956283963589470, -8.104443761338727015, -48.08251050686958905 ) ) ;
#8100 = CARTESIAN_POINT ( 'NONE',  ( -16.99999999999998579, -12.24929059928630437, 38.00000000000012079 ) ) ;
#8101 = EDGE_LOOP ( 'NONE', ( #7981, #14151 ) ) ;
#8102 = CARTESIAN_POINT ( 'NONE',  ( 62.50543674585744469, -2.249290599286311032, 38.00000000000012079 ) ) ;
#8103 = FACE_OUTER_BOUND ( 'NONE', #3582, .T. ) ;
#8104 = EDGE_CURVE ( 'NONE', #11686, #9304, #4340, .T. ) ;
#8105 = ADVANCED_FACE ( 'NONE', ( #11813 ), #7352, .F. ) ;
#8106 = DIRECTION ( 'NONE',  ( 1.000000000000000000, 0.000000000000000000, 0.000000000000000000 ) ) ;
#8107 = DIRECTION ( 'NONE',  ( -1.000000000000000000, 0.000000000000000000, 0.000000000000000000 ) ) ;
#8108 = DIRECTION ( 'NONE',  ( -0.000000000000000000, 0.000000000000000000, 1.000000000000000000 ) ) ;
#8109 = AXIS2_PLACEMENT_3D ( 'NONE', #6618, #11166, #13547 ) ;
#8110 = CARTESIAN_POINT ( 'NONE',  ( 18.00000000000001066, 23.25070940071368497, 33.00000000000012790 ) ) ;
#8111 = ADVANCED_FACE ( 'NONE', ( #10672 ), #6212, .T. ) ;
#8112 = VERTEX_POINT ( 'NONE', #9599 ) ;
#8113 = CARTESIAN_POINT ( 'NONE',  ( 32.84656685061834480, -60.07159297390028030, 1.862767969485127573 ) ) ;
#8114 = ORIENTED_EDGE ( 'NONE', *, *, #13641, .T. ) ;
#8115 = CARTESIAN_POINT ( 'NONE',  ( 8.091875466796944139, -56.38350807138599663, -1.850427664022518348 ) ) ;
#8116 = CARTESIAN_POINT ( 'NONE',  ( 8.091875466796944139, -56.52532528994245808, 1.842181053809107238 ) ) ;
#8117 = ORIENTED_EDGE ( 'NONE', *, *, #10001, .F. ) ;
#8118 = LINE ( 'NONE', #10660, #8442 ) ;
#8119 = CARTESIAN_POINT ( 'NONE',  ( -7.999999999999986677, -2.249290599286305259, -47.50000000000012079 ) ) ;
#8120 = AXIS2_PLACEMENT_3D ( 'NONE', #11310, #925, #5486 ) ;
#8121 = SURFACE_STYLE_USAGE ( .BOTH. , #6967 ) ;
#8122 = CARTESIAN_POINT ( 'NONE',  ( -5.040221427466046400, 4.089237592873870675, 48.00000000000012079 ) ) ;
#8123 = DIRECTION ( 'NONE',  ( 0.000000000000000000, 1.000000000000000000, 0.000000000000000000 ) ) ;
#8124 = CARTESIAN_POINT ( 'NONE',  ( 76.63070922904938698, -6.859691020777852977, 75.19766410831374515 ) ) ;
#8125 = FACE_OUTER_BOUND ( 'NONE', #12385, .T. ) ;
#8126 = EDGE_CURVE ( 'NONE', #14644, #9571, #3733, .T. ) ;
#8127 = CARTESIAN_POINT ( 'NONE',  ( -24.12883632398703782, 3.619414784477793301, -48.08465436988272756 ) ) ;
#8128 = AXIS2_PLACEMENT_3D ( 'NONE', #5335, #5567, #2869 ) ;
#8129 = VERTEX_POINT ( 'NONE', #52 ) ;
#8130 = LINE ( 'NONE', #14976, #7551 ) ;
#8131 = ORIENTED_EDGE ( 'NONE', *, *, #10022, .F. ) ;
#8132 = CARTESIAN_POINT ( 'NONE',  ( -16.99999999999998579, -2.249290599286303927, 50.50000000000012079 ) ) ;
#8133 = ORIENTED_EDGE ( 'NONE', *, *, #902, .T. ) ;
#8134 = SURFACE_STYLE_FILL_AREA ( #6897 ) ;
#8135 = EDGE_LOOP ( 'NONE', ( #6993, #8840, #8980, #1848 ) ) ;
#8136 = CARTESIAN_POINT ( 'NONE',  ( 0.000000000000000000, 21.75070940071369918, 139.1143251403882459 ) ) ;
#8137 = CARTESIAN_POINT ( 'NONE',  ( 103.2469880950108063, 21.75070940071363168, 139.1143251403882459 ) ) ;
#8138 = VECTOR ( 'NONE', #6888, 1000.000000000000000 ) ;
#8139 = CARTESIAN_POINT ( 'NONE',  ( 23.55360291105711212, -55.94205978621073427, -6.462225911923639821 ) ) ;
#8140 = ORIENTED_EDGE ( 'NONE', *, *, #1031, .F. ) ;
#8141 = DIRECTION ( 'NONE',  ( 0.000000000000000000, 0.000000000000000000, -1.000000000000000000 ) ) ;
#8142 = CARTESIAN_POINT ( 'NONE',  ( 8.741820846485476082, -56.83281747056007305, -2.758293468456926245 ) ) ;
#8143 = FACE_OUTER_BOUND ( 'NONE', #13211, .T. ) ;
#8144 = CIRCLE ( 'NONE', #1510, 4.000000000000003553 ) ;
#8145 = EDGE_CURVE ( 'NONE', #13687, #5691, #10575, .T. ) ;
#8146 = EDGE_CURVE ( 'NONE', #6460, #9928, #14434, .T. ) ;
#8147 = CARTESIAN_POINT ( 'NONE',  ( -12.14523415828302078, -9.827631355817260328, 48.50000000000012079 ) ) ;
#8148 = ORIENTED_EDGE ( 'NONE', *, *, #14675, .F. ) ;
#8149 = VECTOR ( 'NONE', #11122, 1000.000000000000000 ) ;
#8150 = EDGE_LOOP ( 'NONE', ( #460, #2090, #576, #1672 ) ) ;
#8151 = AXIS2_PLACEMENT_3D ( 'NONE', #992, #9317, #7859 ) ;
#8152 = DIRECTION ( 'NONE',  ( 1.000000000000000000, 0.000000000000000000, 0.000000000000000000 ) ) ;
#8153 = ORIENTED_EDGE ( 'NONE', *, *, #7723, .T. ) ;
#8154 = CARTESIAN_POINT ( 'NONE',  ( 9.766114723250986174, -60.25982778069332824, -2.890715052751949177 ) ) ;
#8155 = ORIENTED_EDGE ( 'NONE', *, *, #4132, .F. ) ;
#8156 = VERTEX_POINT ( 'NONE', #13412 ) ;
#8157 = TOROIDAL_SURFACE ( 'NONE', #1521, 4.165819364273509962, 0.5000000000000000000 ) ;
#8158 = CARTESIAN_POINT ( 'NONE',  ( -2.688903428702175252E-15, 23.25070940071368142, -33.00000000000012790 ) ) ;
#8159 = DIRECTION ( 'NONE',  ( 1.000000000000000000, 0.000000000000000000, -0.000000000000000000 ) ) ;
#8160 = ORIENTED_EDGE ( 'NONE', *, *, #12524, .T. ) ;
#8161 = AXIS2_PLACEMENT_3D ( 'NONE', #2834, #9927, #455 ) ;
#8162 = VECTOR ( 'NONE', #15090, 1000.000000000000000 ) ;
#8163 = DIRECTION ( 'NONE',  ( -0.000000000000000000, -0.000000000000000000, -1.000000000000000000 ) ) ;
#8164 = CARTESIAN_POINT ( 'NONE',  ( 70.14622571237704562, -3.746881330724391557, 72.37272573528950659 ) ) ;
#8165 = ORIENTED_EDGE ( 'NONE', *, *, #9454, .T. ) ;
#8166 = ADVANCED_FACE ( 'NONE', ( #8578 ), #12413, .F. ) ;
#8167 = DIRECTION ( 'NONE',  ( 1.224646799147353207E-16, 1.000000000000000000, 0.000000000000000000 ) ) ;
#8168 = CARTESIAN_POINT ( 'NONE',  ( -65.00000000000001421, -85.24929059928629727, -19.99999999999999645 ) ) ;
#8169 = ADVANCED_FACE ( 'NONE', ( #6561 ), #709, .F. ) ;
#8170 = DIRECTION ( 'NONE',  ( -0.8208219420614808470, 0.4549890321264226656, 0.3453061251629923611 ) ) ;
#8171 = CARTESIAN_POINT ( 'NONE',  ( 34.73540223981435560, -48.72530132311712237, 2.733088102166433053 ) ) ;
#8172 = ORIENTED_EDGE ( 'NONE', *, *, #14499, .F. ) ;
#8173 =( GEOMETRIC_REPRESENTATION_CONTEXT ( 3 ) GLOBAL_UNCERTAINTY_ASSIGNED_CONTEXT ( ( #2729 ) ) GLOBAL_UNIT_ASSIGNED_CONTEXT ( ( #6118, #13118, #1636 ) ) REPRESENTATION_CONTEXT ( 'NONE', 'WORKASPACE' ) );
#8174 = CARTESIAN_POINT ( 'NONE',  ( 16.55200847196253022, -52.24929059928630437, 4.731961142181928537 ) ) ;
#8175 = VECTOR ( 'NONE', #11407, 1000.000000000000000 ) ;
#8176 = AXIS2_PLACEMENT_3D ( 'NONE', #13634, #776, #3403 ) ;
#8177 = ORIENTED_EDGE ( 'NONE', *, *, #6046, .F. ) ;
#8178 = FACE_OUTER_BOUND ( 'NONE', #1290, .T. ) ;
#8179 = DIRECTION ( 'NONE',  ( -0.000000000000000000, 0.000000000000000000, 1.000000000000000000 ) ) ;
#8180 = ORIENTED_EDGE ( 'NONE', *, *, #4763, .F. ) ;
#8181 = DIRECTION ( 'NONE',  ( -1.000000000000000000, 0.000000000000000000, 0.000000000000000000 ) ) ;
#8182 = DIRECTION ( 'NONE',  ( 0.8746197071345572782, -0.4848096202550659650, 0.000000000000000000 ) ) ;
#8183 = DIRECTION ( 'NONE',  ( -0.000000000000000000, 0.000000000000000000, -1.000000000000000000 ) ) ;
#8184 = VERTEX_POINT ( 'NONE', #5189 ) ;
#8185 = CARTESIAN_POINT ( 'NONE',  ( -26.99999999999998934, -2.249290599286302150, -115.4621125123531442 ) ) ;
#8186 = AXIS2_PLACEMENT_3D ( 'NONE', #10710, #5017, #9722 ) ;
#8187 = CARTESIAN_POINT ( 'NONE',  ( 31.72322230991231962, -61.42570632716525125, -2.132522520905367092 ) ) ;
#8188 = VECTOR ( 'NONE', #757, 1000.000000000000000 ) ;
#8189 = DIRECTION ( 'NONE',  ( 0.000000000000000000, 0.000000000000000000, 1.000000000000000000 ) ) ;
#8190 = LINE ( 'NONE', #12892, #2448 ) ;
#8191 = CIRCLE ( 'NONE', #12607, 7.000000000000000000 ) ;
#8192 = DIRECTION ( 'NONE',  ( 0.8656763553493062036, 0.5006040828730242698, 0.000000000000000000 ) ) ;
#8193 = DIRECTION ( 'NONE',  ( -0.3020115420618248447, 0.1674077314120184512, -0.9384901064608619503 ) ) ;
#8194 = EDGE_CURVE ( 'NONE', #4644, #15071, #14576, .T. ) ;
#8195 = ORIENTED_EDGE ( 'NONE', *, *, #6946, .F. ) ;
#8196 = ORIENTED_EDGE ( 'NONE', *, *, #1084, .T. ) ;
#8197 = LINE ( 'NONE', #7031, #7370 ) ;
#8198 = ORIENTED_EDGE ( 'NONE', *, *, #8772, .F. ) ;
#8199 = ADVANCED_FACE ( 'NONE', ( #11111 ), #2809, .T. ) ;
#8200 = FACE_OUTER_BOUND ( 'NONE', #10743, .T. ) ;
#8201 = CARTESIAN_POINT ( 'NONE',  ( 17.61519226005271577, -69.39711819508849544, 6.201611931792121446 ) ) ;
#8202 = EDGE_CURVE ( 'NONE', #1125, #8531, #4173, .T. ) ;
#8203 = VECTOR ( 'NONE', #11434, 1000.000000000000000 ) ;
#8204 = ORIENTED_EDGE ( 'NONE', *, *, #12039, .F. ) ;
#8205 = LINE ( 'NONE', #2577, #1878 ) ;
#8206 = CARTESIAN_POINT ( 'NONE',  ( -9.037775043065352065, 2.932694901963889489, 58.00000000000012079 ) ) ;
#8207 = DIRECTION ( 'NONE',  ( -0.000000000000000000, -0.000000000000000000, -1.000000000000000000 ) ) ;
#8208 = ADVANCED_FACE ( 'NONE', ( #3884 ), #491, .F. ) ;
#8209 = ADVANCED_FACE ( 'NONE', ( #9891 ), #14144, .F. ) ;
#8210 = CARTESIAN_POINT ( 'NONE',  ( 50.07597535787931520, -2.249290599286309256, 48.51982618741349285 ) ) ;
#8211 = CARTESIAN_POINT ( 'NONE',  ( 54.03086304124234829, 0.8903401505190762233, 60.61639468829817190 ) ) ;
#8212 = CARTESIAN_POINT ( 'NONE',  ( 61.57572300660984865, -8.804762498903286883, 76.19766410831374515 ) ) ;
#8213 = CARTESIAN_POINT ( 'NONE',  ( 14.04997225853032461, -69.39711819508849544, 4.211076768700158013 ) ) ;
#8214 = CARTESIAN_POINT ( 'NONE',  ( 32.29311415220630721, -54.59388862152662369, 3.160229925968714770 ) ) ;
#8215 = CIRCLE ( 'NONE', #10634, 31.00000000000000000 ) ;
#8216 = ADVANCED_FACE ( 'NONE', ( #8033 ), #5653, .T. ) ;
#8217 = ORIENTED_EDGE ( 'NONE', *, *, #1040, .F. ) ;
#8218 = PLANE ( 'NONE',  #177 ) ;
#8219 = ORIENTED_EDGE ( 'NONE', *, *, #14946, .T. ) ;
#8220 = EDGE_CURVE ( 'NONE', #4043, #211, #12575, .T. ) ;
#8221 = DIRECTION ( 'NONE',  ( -0.7152862910730209967, -0.6988315403607663345, 0.000000000000000000 ) ) ;
#8222 = VERTEX_POINT ( 'NONE', #12650 ) ;
#8223 = ADVANCED_FACE ( 'NONE', ( #5573 ), #7804, .F. ) ;
#8224 = ORIENTED_EDGE ( 'NONE', *, *, #12062, .T. ) ;
#8225 = CARTESIAN_POINT ( 'NONE',  ( 65.27061521436114333, -11.12190849844603058, 76.21551869727603901 ) ) ;
#8226 = DIRECTION ( 'NONE',  ( 0.8746197071345573892, -0.4848096202550657985, 0.000000000000000000 ) ) ;
#8227 = CARTESIAN_POINT ( 'NONE',  ( 18.24487436548682950, -53.24929059928630437, -6.492462156583997945 ) ) ;
#8228 = ORIENTED_EDGE ( 'NONE', *, *, #1010, .F. ) ;
#8229 = EDGE_LOOP ( 'NONE', ( #10518, #4572, #13923, #9566 ) ) ;
#8230 = CARTESIAN_POINT ( 'NONE',  ( 8.332112475568445475, -58.05408529505832149, -2.501672671511202761 ) ) ;
#8231 = CARTESIAN_POINT ( 'NONE',  ( 53.11142512232702018, -3.558169932106523881, 60.61639468829817190 ) ) ;
#8232 = FACE_OUTER_BOUND ( 'NONE', #13725, .T. ) ;
#8233 = ORIENTED_EDGE ( 'NONE', *, *, #5591, .F. ) ;
#8234 = VERTEX_POINT ( 'NONE', #2099 ) ;
#8235 = DIRECTION ( 'NONE',  ( -0.000000000000000000, -0.000000000000000000, -1.000000000000000000 ) ) ;
#8236 = VERTEX_POINT ( 'NONE', #4326 ) ;
#8237 = CARTESIAN_POINT ( 'NONE',  ( 9.287096315897038323, -59.39117099671924649, -2.764779704643934188 ) ) ;
#8238 = ORIENTED_EDGE ( 'NONE', *, *, #1738, .T. ) ;
#8239 = ORIENTED_EDGE ( 'NONE', *, *, #13085, .T. ) ;
#8240 = ADVANCED_FACE ( 'NONE', ( #1098 ), #2025, .F. ) ;
#8241 = LINE ( 'NONE', #8158, #2119 ) ;
#8242 = DIRECTION ( 'NONE',  ( 0.000000000000000000, -0.000000000000000000, -1.000000000000000000 ) ) ;
#8243 = ADVANCED_FACE ( 'NONE', ( #6719 ), #13631, .T. ) ;
#8244 = DIRECTION ( 'NONE',  ( 0.000000000000000000, 0.000000000000000000, -1.000000000000000000 ) ) ;
#8245 = FACE_OUTER_BOUND ( 'NONE', #14090, .T. ) ;
#8246 = ORIENTED_EDGE ( 'NONE', *, *, #3581, .F. ) ;
#8247 = DIRECTION ( 'NONE',  ( 0.000000000000000000, 0.000000000000000000, 1.000000000000000000 ) ) ;
#8248 = DIRECTION ( 'NONE',  ( 0.8420378618367651002, 0.5394184268574528929, -2.807225425332302624E-15 ) ) ;
#8249 = FACE_OUTER_BOUND ( 'NONE', #5652, .T. ) ;
#8250 = CARTESIAN_POINT ( 'NONE',  ( 114.0000000000000284, 19.25070940071369563, 13.14990448602693007 ) ) ;
#8251 = ORIENTED_EDGE ( 'NONE', *, *, #5886, .T. ) ;
#8252 = DIRECTION ( 'NONE',  ( -0.8908241094534361526, -0.4543483311474716957, 0.000000000000000000 ) ) ;
#8253 = ORIENTED_EDGE ( 'NONE', *, *, #5136, .F. ) ;
#8254 = DIRECTION ( 'NONE',  ( -1.734723475976807292E-15, 1.000000000000000000, 0.000000000000000000 ) ) ;
#8255 = CARTESIAN_POINT ( 'NONE',  ( 53.54504563787001814, -4.650271872399136086, 62.84860122826521689 ) ) ;
#8256 = ORIENTED_EDGE ( 'NONE', *, *, #6313, .T. ) ;
#8257 = EDGE_CURVE ( 'NONE', #3688, #2288, #11050, .T. ) ;
#8258 = ADVANCED_FACE ( 'NONE', ( #5502 ), #10112, .T. ) ;
#8259 = ORIENTED_EDGE ( 'NONE', *, *, #5459, .T. ) ;
#8260 = DIRECTION ( 'NONE',  ( 1.000000000000000000, 0.000000000000000000, 0.000000000000000000 ) ) ;
#8261 = CARTESIAN_POINT ( 'NONE',  ( 8.821484763567292831, -57.33450387999030795, 2.749014434309880794 ) ) ;
#8262 = CARTESIAN_POINT ( 'NONE',  ( 118.0000000000000284, 19.25070940071370273, 33.00000000000012790 ) ) ;
#8263 = ORIENTED_EDGE ( 'NONE', *, *, #3559, .T. ) ;
#8264 = VERTEX_POINT ( 'NONE', #6641 ) ;
#8265 = DIRECTION ( 'NONE',  ( 0.5394184268574402363, -0.8420378618367729828, 0.000000000000000000 ) ) ;
#8266 = CARTESIAN_POINT ( 'NONE',  ( 32.06582363241078326, -61.15506547911481050, -2.039555069692439382 ) ) ;
#8267 = FACE_OUTER_BOUND ( 'NONE', #5384, .T. ) ;
#8268 = CARTESIAN_POINT ( 'NONE',  ( 82.49066175147797253, 12.46743062497963450, 33.00000000000014211 ) ) ;
#8269 = CARTESIAN_POINT ( 'NONE',  ( -24.60511756109301373, -7.062218017875619758, -48.00656353678737531 ) ) ;
#8270 = CARTESIAN_POINT ( 'NONE',  ( 58.00000000000000711, 10.75070940071368852, -33.00000000000012790 ) ) ;
#8271 = ORIENTED_EDGE ( 'NONE', *, *, #14983, .F. ) ;
#8272 = AXIS2_PLACEMENT_3D ( 'NONE', #2931, #4223, #3930 ) ;
#8273 = LINE ( 'NONE', #14349, #13756 ) ;
#8274 = ORIENTED_EDGE ( 'NONE', *, *, #8518, .T. ) ;
#8275 = CARTESIAN_POINT ( 'NONE',  ( 27.86173033120691045, -69.39711819508849544, 2.500000000000000000 ) ) ;
#8276 = DIRECTION ( 'NONE',  ( 0.000000000000000000, 0.000000000000000000, 1.000000000000000000 ) ) ;
#8277 = DIRECTION ( 'NONE',  ( -0.8656763553492640151, -0.5006040828730974335, 0.000000000000000000 ) ) ;
#8278 = CARTESIAN_POINT ( 'NONE',  ( 9.175559494770816116, -57.26105658658105568, 1.816685854991392013 ) ) ;
#8279 = LINE ( 'NONE', #4517, #7543 ) ;
#8280 = CARTESIAN_POINT ( 'NONE',  ( 104.0000000000000426, 11.25070940071369563, 33.00000000000012790 ) ) ;
#8281 = AXIS2_PLACEMENT_3D ( 'NONE', #1747, #14389, #2763 ) ;
#8282 = AXIS2_PLACEMENT_3D ( 'NONE', #5796, #14175, #2242 ) ;
#8283 = DIRECTION ( 'NONE',  ( 0.000000000000000000, 0.000000000000000000, 1.000000000000000000 ) ) ;
#8284 = CARTESIAN_POINT ( 'NONE',  ( -24.85140262670387301, -6.666068128078234345, 48.18452149279842445 ) ) ;
#8285 = CARTESIAN_POINT ( 'NONE',  ( 9.764632533060700226, -60.25800154558400834, 2.890242835725739479 ) ) ;
#8286 = CARTESIAN_POINT ( 'NONE',  ( 32.85196700223596622, -54.05847863454827262, 2.186919301701788054 ) ) ;
#8287 = ADVANCED_FACE ( 'NONE', ( #3180 ), #789, .T. ) ;
#8288 = ORIENTED_EDGE ( 'NONE', *, *, #10463, .T. ) ;
#8289 = CARTESIAN_POINT ( 'NONE',  ( 0.000000000000000000, 21.75070940071356418, 33.00000000000012790 ) ) ;
#8290 = UNCERTAINTY_MEASURE_WITH_UNIT (LENGTH_MEASURE( 1.000000000000000082E-05 ), #8710, 'distance_accuracy_value', 'NONE');
#8291 = ORIENTED_EDGE ( 'NONE', *, *, #1194, .F. ) ;
#8292 = EDGE_CURVE ( 'NONE', #117, #13103, #10070, .T. ) ;
#8293 = CARTESIAN_POINT ( 'NONE',  ( 16.19117549353424579, -53.25924485586082113, 5.664696970550274102 ) ) ;
#8294 = AXIS2_PLACEMENT_3D ( 'NONE', #194, #14125, #9591 ) ;
#8295 = ORIENTED_EDGE ( 'NONE', *, *, #3022, .F. ) ;
#8296 = AXIS2_PLACEMENT_3D ( 'NONE', #14511, #8658, #12501 ) ;
#8297 = ORIENTED_EDGE ( 'NONE', *, *, #3677, .F. ) ;
#8298 = CARTESIAN_POINT ( 'NONE',  ( 65.13162939602318602, -11.91918766459985335, 75.19766410831374515 ) ) ;
#8299 = CYLINDRICAL_SURFACE ( 'NONE', #7052, 11.46463184759105403 ) ;
#8300 = CARTESIAN_POINT ( 'NONE',  ( 14.12076545371522229, -53.27034158699088806, -4.884662653952329237 ) ) ;
#8301 = AXIS2_PLACEMENT_3D ( 'NONE', #9748, #1427, #1504 ) ;
#8302 = CARTESIAN_POINT ( 'NONE',  ( 8.863084284310778216, -54.05488119003518221, 2.185023599737856870 ) ) ;
#8303 = CIRCLE ( 'NONE', #10015, 0.5000000000000004441 ) ;
#8304 = EDGE_CURVE ( 'NONE', #56, #4994, #7865, .T. ) ;
#8305 = ADVANCED_FACE ( 'NONE', ( #7260 ), #1227, .T. ) ;
#8306 = CIRCLE ( 'NONE', #10999, 4.665819364273509073 ) ;
#8307 = FACE_OUTER_BOUND ( 'NONE', #8598, .T. ) ;
#8308 = DIRECTION ( 'NONE',  ( 0.000000000000000000, 0.000000000000000000, 1.000000000000000000 ) ) ;
#8309 = ORIENTED_EDGE ( 'NONE', *, *, #13014, .F. ) ;
#8310 = ORIENTED_EDGE ( 'NONE', *, *, #6594, .T. ) ;
#8311 = CARTESIAN_POINT ( 'NONE',  ( -1.197457146693678531, -2.220571218158920779, -48.00000000000012079 ) ) ;
#8312 = EDGE_LOOP ( 'NONE', ( #2813, #6217, #10221, #4279 ) ) ;
#8313 = LINE ( 'NONE', #4916, #10387 ) ;
#8314 = VECTOR ( 'NONE', #219, 1000.000000000000000 ) ;
#8315 = EDGE_LOOP ( 'NONE', ( #13433, #4758, #9639, #15039 ) ) ;
#8316 = CARTESIAN_POINT ( 'NONE',  ( 12.02094163398139237, -52.24929059928630437, 4.175384597093461103 ) ) ;
#8317 = AXIS2_PLACEMENT_3D ( 'NONE', #8808, #12426, #7511 ) ;
#8318 = ORIENTED_EDGE ( 'NONE', *, *, #1519, .T. ) ;
#8319 = CIRCLE ( 'NONE', #10530, 3.694885682587998765 ) ;
#8320 = VECTOR ( 'NONE', #5560, 1000.000000000000000 ) ;
#8321 = CARTESIAN_POINT ( 'NONE',  ( -22.41471376588497222, 4.941665658445489662, -48.26816462195809265 ) ) ;
#8322 = CARTESIAN_POINT ( 'NONE',  ( 55.08546260466144417, 2.477934215446290445, 54.56811043785582882 ) ) ;
#8323 = ORIENTED_EDGE ( 'NONE', *, *, #5626, .T. ) ;
#8324 = APPLICATION_CONTEXT ( 'automotive_design' ) ;
#8325 = DIRECTION ( 'NONE',  ( 1.000000000000000000, 0.000000000000000000, 0.000000000000000000 ) ) ;
#8326 = FACE_OUTER_BOUND ( 'NONE', #14902, .T. ) ;
#8327 = EDGE_LOOP ( 'NONE', ( #7383, #6941 ) ) ;
#8328 = DIRECTION ( 'NONE',  ( -1.000000000000000000, 0.000000000000000000, 0.000000000000000000 ) ) ;
#8329 = DIRECTION ( 'NONE',  ( 0.000000000000000000, 0.000000000000000000, 1.000000000000000000 ) ) ;
#8330 = DIRECTION ( 'NONE',  ( 0.000000000000000000, 0.000000000000000000, -1.000000000000000000 ) ) ;
#8331 = ORIENTED_EDGE ( 'NONE', *, *, #9993, .F. ) ;
#8332 = DIRECTION ( 'NONE',  ( 0.000000000000000000, 0.000000000000000000, 1.000000000000000000 ) ) ;
#8333 = EDGE_CURVE ( 'NONE', #59, #2925, #13275, .T. ) ;
#8334 = EDGE_LOOP ( 'NONE', ( #15150, #772, #12618, #14193 ) ) ;
#8335 = CYLINDRICAL_SURFACE ( 'NONE', #13080, 2.499999999999995115 ) ;
#8336 = ORIENTED_EDGE ( 'NONE', *, *, #8388, .F. ) ;
#8337 = ORIENTED_EDGE ( 'NONE', *, *, #7246, .T. ) ;
#8338 = DIRECTION ( 'NONE',  ( 0.000000000000000000, 0.000000000000000000, 1.000000000000000000 ) ) ;
#8339 = DIRECTION ( 'NONE',  ( 0.5394184268574520047, -0.8420378618367654333, 0.000000000000000000 ) ) ;
#8340 = DIRECTION ( 'NONE',  ( -0.000000000000000000, 1.000000000000000000, 1.445602896647339163E-16 ) ) ;
#8341 = CARTESIAN_POINT ( 'NONE',  ( 31.74727030611957446, -60.51242536180950538, -2.958269724472593065 ) ) ;
#8342 = B_SPLINE_CURVE_WITH_KNOTS ( 'NONE', 3,
 ( #12245, #13469, #7623, #611, #3307, #10162, #12785, #7775, #3228, #10233, #9167, #835, #11448, #6842, #913, #14847, #13852, #5544 ),
 .UNSPECIFIED., .F., .F.,
 ( 4, 2, 2, 2, 2, 2, 2, 2, 4 ),
 ( 0.000000000000000000, 0.0007591815323294849030, 0.001518363064658969806, 0.002277544596988454600, 0.003036726129317939612, 0.003795907661647424623, 0.004555089193976909201, 0.005314270726306394646, 0.006073452258635879224 ),
 .UNSPECIFIED. ) ;
#8343 = ADVANCED_BREP_SHAPE_REPRESENTATION ( '', ( #4097, #6315 ), #2129 ) ;
#8344 = CARTESIAN_POINT ( 'NONE',  ( 0.5043391135745837195, 0.8906624217387615339, -57.50000000000012079 ) ) ;
#8345 = DIRECTION ( 'NONE',  ( -0.8746197071345569451, 0.4848096202550666312, 0.000000000000000000 ) ) ;
#8346 = LINE ( 'NONE', #8561, #1551 ) ;
#8347 = CARTESIAN_POINT ( 'NONE',  ( 33.25220092076087752, -54.75705460292245164, -2.044066819204659602 ) ) ;
#8348 = EDGE_CURVE ( 'NONE', #10484, #11185, #5401, .T. ) ;
#8349 =( BOUNDED_SURFACE ( )  B_SPLINE_SURFACE ( 3, 2, ( 
 ( #7684, #13376, #8825 ),
 ( #12297, #6448, #5222 ),
 ( #7605, #14602, #5073 ),
 ( #4050, #8748, #312 ),
 ( #5296, #13446, #5004 ),
 ( #3910, #2909, #7466 ),
 ( #9710, #14392, #3834 ),
 ( #8541, #2686, #7386 ),
 ( #12076, #1540, #6246 ),
 ( #8607, #2768, #12154 ),
 ( #1608, #6303, #10998 ),
 ( #5145, #9852, #9145 ),
 ( #14750, #11429, #11511 ),
 ( #11280, #4202, #4436 ) ),
 .UNSPECIFIED., .F., .F., .F. ) 
 B_SPLINE_SURFACE_WITH_KNOTS ( ( 4, 2, 2, 2, 2, 2, 4 ),
 ( 3, 3 ),
 ( 0.000000000000000000, 0.002560658414910377267, 0.003840987622365565901, 0.005121316829820754535, 0.006401646037275943169, 0.007681975244731131802, 0.01024263365964150907 ),
 ( 0.000000000000000000, 1.000000000000000000 ),
 .UNSPECIFIED. ) 
 GEOMETRIC_REPRESENTATION_ITEM ( )  RATIONAL_B_SPLINE_SURFACE ( (
 ( 1.000000000000000000, 0.8053615646146050633, 1.000000000000000000),
 ( 1.000000000000000000, 0.8105996499491056051, 1.000000000000000000),
 ( 1.000000000000000000, 0.8160199193853731048, 1.000000000000000000),
 ( 1.000000000000000000, 0.8240376314735113894, 1.000000000000000000),
 ( 1.000000000000000000, 0.8266971106456140195, 1.000000000000000000),
 ( 1.000000000000000000, 0.8319110421176807435, 1.000000000000000000),
 ( 1.000000000000000000, 0.8344214672179540715, 1.000000000000000000),
 ( 1.000000000000000000, 0.8392107060237447014, 1.000000000000000000),
 ( 1.000000000000000000, 0.8414897010533705091, 1.000000000000000000),
 ( 1.000000000000000000, 0.8457750297008398421, 1.000000000000000000),
 ( 1.000000000000000000, 0.8477871175334191767, 1.000000000000000000),
 ( 1.000000000000000000, 0.8533050377659211483, 1.000000000000000000),
 ( 1.000000000000000000, 0.8561733496717631731, 1.000000000000000000),
 ( 1.000000000000000000, 0.8581891718822901582, 1.000000000000000000) ) ) 
 REPRESENTATION_ITEM ( '' )  SURFACE ( )  );
#8350 = ORIENTED_EDGE ( 'NONE', *, *, #14929, .F. ) ;
#8351 = CARTESIAN_POINT ( 'NONE',  ( 25.81270058232203013, 21.75070940071309167, 33.00000000000012790 ) ) ;
#8352 = EDGE_LOOP ( 'NONE', ( #12333, #4470, #2075, #2876, #8387 ) ) ;
#8353 = DIRECTION ( 'NONE',  ( 1.156482317317870492E-16, -1.000000000000000000, 0.000000000000000000 ) ) ;
#8354 = FACE_OUTER_BOUND ( 'NONE', #13717, .T. ) ;
#8355 = DIRECTION ( 'NONE',  ( -0.000000000000000000, -0.000000000000000000, -1.000000000000000000 ) ) ;
#8356 = DIRECTION ( 'NONE',  ( -0.8208219420614786266, 0.4549890321264268844, 0.3453061251629920281 ) ) ;
#8357 = CARTESIAN_POINT ( 'NONE',  ( 70.25043121783370736, -4.317737931693936382, 76.19766410831374515 ) ) ;
#8358 = CARTESIAN_POINT ( 'NONE',  ( 65.22587406926737685, -11.15092874177724980, 71.30368058120426156 ) ) ;
#8359 = VECTOR ( 'NONE', #4460, 1000.000000000000000 ) ;
#8360 = MECHANICAL_DESIGN_GEOMETRIC_PRESENTATION_REPRESENTATION (  '', ( #6378 ), #5648 ) ;
#8361 = CYLINDRICAL_SURFACE ( 'NONE', #7571, 1.000000000000005329 ) ;
#8362 = CARTESIAN_POINT ( 'NONE',  ( -24.99086469133269617, -6.390485686409522081, 48.00342231809331395 ) ) ;
#8363 = EDGE_CURVE ( 'NONE', #5234, #3379, #3650, .T. ) ;
#8364 = DIRECTION ( 'NONE',  ( -0.3738365665314423159, 0.000000000000000000, -0.9274945937977119303 ) ) ;
#8365 = ORIENTED_EDGE ( 'NONE', *, *, #5794, .F. ) ;
#8366 = CARTESIAN_POINT ( 'NONE',  ( 58.14816640453862107, 2.809303687574978614, 60.61639468829817190 ) ) ;
#8367 = ORIENTED_EDGE ( 'NONE', *, *, #13911, .T. ) ;
#8368 = CARTESIAN_POINT ( 'NONE',  ( 35.49198652140812982, 0.000000000000000000, 33.00000000000012790 ) ) ;
#8369 = AXIS2_PLACEMENT_3D ( 'NONE', #13479, #8633, #6399 ) ;
#8370 = ORIENTED_EDGE ( 'NONE', *, *, #4000, .F. ) ;
#8371 = CARTESIAN_POINT ( 'NONE',  ( 65.62087295291071598, -10.81524950655579786, 76.23790561730409365 ) ) ;
#8372 = CARTESIAN_POINT ( 'NONE',  ( 104.9938193859979236, 23.25070940071369208, 33.00000000000012790 ) ) ;
#8373 = CARTESIAN_POINT ( 'NONE',  ( -3.285520523749251520, 5.681530634151883419, 48.50000000000012079 ) ) ;
#8374 = CARTESIAN_POINT ( 'NONE',  ( 9.329831199630714167, -53.50309148220239308, 3.187126068577730287 ) ) ;
#8375 = MECHANICAL_DESIGN_GEOMETRIC_PRESENTATION_REPRESENTATION (  '', ( #13046 ), #8842 ) ;
#8376 = CARTESIAN_POINT ( 'NONE',  ( -24.90998783373886738, 2.881753107372537759, 48.00000000000012079 ) ) ;
#8377 = DIRECTION ( 'NONE',  ( 0.000000000000000000, 1.000000000000000000, 0.000000000000000000 ) ) ;
#8378 = ORIENTED_EDGE ( 'NONE', *, *, #7272, .F. ) ;
#8379 = ORIENTED_EDGE ( 'NONE', *, *, #4601, .F. ) ;
#8380 = CARTESIAN_POINT ( 'NONE',  ( 18.00000000000001066, 23.25070940071368497, 139.1143251403882459 ) ) ;
#8381 = EDGE_CURVE ( 'NONE', #10163, #2925, #4416, .T. ) ;
#8382 = ORIENTED_EDGE ( 'NONE', *, *, #1309, .T. ) ;
#8383 = FACE_OUTER_BOUND ( 'NONE', #2552, .T. ) ;
#8384 = ORIENTED_EDGE ( 'NONE', *, *, #2968, .F. ) ;
#8385 = DIRECTION ( 'NONE',  ( -0.8656763553493062036, -0.5006040828730242698, -0.000000000000000000 ) ) ;
#8386 = AXIS2_PLACEMENT_3D ( 'NONE', #9960, #3032, #3946 ) ;
#8387 = ORIENTED_EDGE ( 'NONE', *, *, #2868, .F. ) ;
#8388 = EDGE_CURVE ( 'NONE', #11544, #2180, #12023, .T. ) ;
#8389 = ADVANCED_FACE ( 'NONE', ( #3794 ), #4159, .F. ) ;
#8390 = EDGE_CURVE ( 'NONE', #9917, #4237, #8197, .T. ) ;
#8391 = CARTESIAN_POINT ( 'NONE',  ( 25.81270058232203013, 23.25070940071368852, -33.00000000000012790 ) ) ;
#8392 = DIRECTION ( 'NONE',  ( -0.000000000000000000, 0.000000000000000000, -1.000000000000000000 ) ) ;
#8393 = ORIENTED_EDGE ( 'NONE', *, *, #9520, .F. ) ;
#8394 = LINE ( 'NONE', #13087, #2993 ) ;
#8395 = CARTESIAN_POINT ( 'NONE',  ( -8.590985667557523797, 2.187759657648595368, 48.00000000000012079 ) ) ;
#8396 = VERTEX_POINT ( 'NONE', #4728 ) ;
#8397 = EDGE_CURVE ( 'NONE', #14241, #77, #8273, .T. ) ;
#8398 = AXIS2_PLACEMENT_3D ( 'NONE', #4388, #13775, #12629 ) ;
#8399 = CARTESIAN_POINT ( 'NONE',  ( 27.33382790127957662, -69.39711819508849544, -4.502057496415715399 ) ) ;
#8400 = CARTESIAN_POINT ( 'NONE',  ( -9.268887740808379405, 2.359106894006888666, -47.70917337021941762 ) ) ;
#8401 = CARTESIAN_POINT ( 'NONE',  ( -7.499999999999985789, -2.249290599286303927, -48.00000000000012079 ) ) ;
#8402 = VERTEX_POINT ( 'NONE', #8351 ) ;
#8403 = CARTESIAN_POINT ( 'NONE',  ( -22.46208338003149407, 4.939996070762163960, 48.38299871081639481 ) ) ;
#8404 = VECTOR ( 'NONE', #5418, 1000.000000000000114 ) ;
#8405 = VERTEX_POINT ( 'NONE', #11797 ) ;
#8406 = VECTOR ( 'NONE', #1146, 1000.000000000000000 ) ;
#8407 = CYLINDRICAL_SURFACE ( 'NONE', #3002, 4.276034690655513337 ) ;
#8408 = LINE ( 'NONE', #3477, #2847 ) ;
#8409 = ORIENTED_EDGE ( 'NONE', *, *, #6585, .F. ) ;
#8410 = AXIS2_PLACEMENT_3D ( 'NONE', #14430, #9300, #9455 ) ;
#8411 = EDGE_CURVE ( 'NONE', #1886, #12128, #10324, .T. ) ;
#8412 = DIRECTION ( 'NONE',  ( 0.000000000000000000, 0.000000000000000000, 1.000000000000000000 ) ) ;
#8413 = CARTESIAN_POINT ( 'NONE',  ( 80.18290120114222930, 25.52935533987996664, -21.00807340887166674 ) ) ;
#8414 = DIRECTION ( 'NONE',  ( 0.000000000000000000, -1.000000000000000000, 0.000000000000000000 ) ) ;
#8415 = DIRECTION ( 'NONE',  ( -0.000000000000000000, -0.000000000000000000, -1.000000000000000000 ) ) ;
#8416 = CARTESIAN_POINT ( 'NONE',  ( 13.69672121530045139, -65.45069003753607717, 4.122770147408488128 ) ) ;
#8417 = VECTOR ( 'NONE', #14630, 1000.000000000000000 ) ;
#8418 = DIRECTION ( 'NONE',  ( -1.000000000000000000, 0.000000000000000000, 0.000000000000000000 ) ) ;
#8419 = CARTESIAN_POINT ( 'NONE',  ( 114.0000000000000284, 19.25070940071369563, 139.1143251403882459 ) ) ;
#8420 = VECTOR ( 'NONE', #7576, 1000.000000000000000 ) ;
#8421 = CARTESIAN_POINT ( 'NONE',  ( -24.89835624542414649, -6.565460432723037698, 47.52815511422343775 ) ) ;
#8422 = CARTESIAN_POINT ( 'NONE',  ( 30.88809549976038582, -52.51002131803713979, -3.753497227305021777 ) ) ;
#8423 = CIRCLE ( 'NONE', #10375, 0.7892041907098262810 ) ;
#8424 = DIRECTION ( 'NONE',  ( -0.000000000000000000, 0.000000000000000000, 1.000000000000000000 ) ) ;
#8425 = ORIENTED_EDGE ( 'NONE', *, *, #3310, .T. ) ;
#8426 = PLANE ( 'NONE',  #42 ) ;
#8427 = LINE ( 'NONE', #9430, #3004 ) ;
#8428 = ADVANCED_FACE ( 'NONE', ( #9427 ), #11878, .T. ) ;
#8429 = EDGE_LOOP ( 'NONE', ( #12537, #2598, #14078, #4683 ) ) ;
#8430 =( GEOMETRIC_REPRESENTATION_CONTEXT ( 3 ) GLOBAL_UNCERTAINTY_ASSIGNED_CONTEXT ( ( #5828 ) ) GLOBAL_UNIT_ASSIGNED_CONTEXT ( ( #8761, #11223, #4590 ) ) REPRESENTATION_CONTEXT ( 'NONE', 'WORKASPACE' ) );
#8431 = CARTESIAN_POINT ( 'NONE',  ( 93.56770215592470663, 21.75070940071356418, 139.1143251403882459 ) ) ;
#8432 = LINE ( 'NONE', #2345, #1160 ) ;
#8433 = VECTOR ( 'NONE', #7596, 999.9999999999998863 ) ;
#8434 = VECTOR ( 'NONE', #394, 1000.000000000000000 ) ;
#8435 = CARTESIAN_POINT ( 'NONE',  ( 69.37744794823258587, -3.711917656928557463, 76.21513011789701864 ) ) ;
#8436 = LINE ( 'NONE', #13126, #9394 ) ;
#8437 = EDGE_CURVE ( 'NONE', #13017, #14235, #13040, .T. ) ;
#8438 = ADVANCED_FACE ( 'NONE', ( #1337 ), #11284, .F. ) ;
#8439 = CIRCLE ( 'NONE', #14330, 10.00000000000000000 ) ;
#8440 = LINE ( 'NONE', #4890, #10769 ) ;
#8441 = CARTESIAN_POINT ( 'NONE',  ( 80.18290120114222930, 23.25070940071369208, 33.00000000000014211 ) ) ;
#8442 = VECTOR ( 'NONE', #190, 1000.000000000000000 ) ;
#8443 = CARTESIAN_POINT ( 'NONE',  ( 31.16597161352219558, -52.62785358159868565, 3.652922677140724605 ) ) ;
#8444 = VERTEX_POINT ( 'NONE', #14268 ) ;
#8445 = AXIS2_PLACEMENT_3D ( 'NONE', #3819, #10915, #8591 ) ;
#8446 = DIRECTION ( 'NONE',  ( 0.000000000000000000, 0.000000000000000000, 1.000000000000000000 ) ) ;
#8447 = VECTOR ( 'NONE', #13141, 1000.000000000000000 ) ;
#8448 = VERTEX_POINT ( 'NONE', #13116 ) ;
#8449 = DIRECTION ( 'NONE',  ( 0.000000000000000000, 0.000000000000000000, -1.000000000000000000 ) ) ;
#8450 = ORIENTED_EDGE ( 'NONE', *, *, #11499, .T. ) ;
#8451 = B_SPLINE_CURVE_WITH_KNOTS ( 'NONE', 3,
 ( #8629, #11304, #12630, #5629, #11534, #7936, #6695, #3082, #2077, #13706, #10238, #993, #6767, #14931, #10089, #7707, #11233, #3313 ),
 .UNSPECIFIED., .F., .F.,
 ( 4, 2, 2, 2, 2, 2, 2, 2, 4 ),
 ( 0.000000000000000000, 0.0003958370570530562473, 0.0007916741141061124946, 0.001187511171159168688, 0.001583348228212224989, 0.001979185285265281074, 0.002375022342318337375, 0.002770859399371394111, 0.003166696456424448677 ),
 .UNSPECIFIED. ) ;
#8452 = ORIENTED_EDGE ( 'NONE', *, *, #14320, .F. ) ;
#8453 = CARTESIAN_POINT ( 'NONE',  ( 82.49066175147797253, 12.46743062497963450, 84.20452624982236500 ) ) ;
#8454 = DIRECTION ( 'NONE',  ( 0.000000000000000000, 0.000000000000000000, 1.000000000000000000 ) ) ;
#8455 = EDGE_CURVE ( 'NONE', #10777, #7767, #10804, .T. ) ;
#8456 = ADVANCED_FACE ( 'NONE', ( #13186 ), #7620, .T. ) ;
#8457 = DIRECTION ( 'NONE',  ( 0.000000000000000000, 1.000000000000000000, -0.000000000000000000 ) ) ;
#8458 = CIRCLE ( 'NONE', #9921, 0.5000000000000008882 ) ;
#8459 = EDGE_LOOP ( 'NONE', ( #13428, #10113, #3316, #3679 ) ) ;
#8460 = VECTOR ( 'NONE', #7161, 1000.000000000000000 ) ;
#8461 = CARTESIAN_POINT ( 'NONE',  ( -23.85820543185402798, 3.853856159079054322, 48.12676452506695313 ) ) ;
#8462 = LINE ( 'NONE', #8523, #8768 ) ;
#8463 = ORIENTED_EDGE ( 'NONE', *, *, #14674, .F. ) ;
#8464 = ORIENTED_EDGE ( 'NONE', *, *, #5917, .T. ) ;
#8465 = DIRECTION ( 'NONE',  ( 0.000000000000000000, -0.000000000000000000, 1.000000000000000000 ) ) ;
#8466 = ORIENTED_EDGE ( 'NONE', *, *, #7252, .F. ) ;
#8467 = LINE ( 'NONE', #2603, #13061 ) ;
#8468 = VERTEX_POINT ( 'NONE', #12108 ) ;
#8469 = CARTESIAN_POINT ( 'NONE',  ( 29.24282639220357538, -63.10178406536851270, 3.876738539649118298 ) ) ;
#8470 = ORIENTED_EDGE ( 'NONE', *, *, #3115, .F. ) ;
#8471 = CARTESIAN_POINT ( 'NONE',  ( 20.86173033120691045, -52.24929059928630437, -7.000000000000000000 ) ) ;
#8472 = CARTESIAN_POINT ( 'NONE',  ( -10.31873516982594907, -8.289185193041582522, 47.74939190649462972 ) ) ;
#8473 = EDGE_LOOP ( 'NONE', ( #7460, #7519, #14460, #9754 ) ) ;
#8474 = CARTESIAN_POINT ( 'NONE',  ( 0.000000000000000000, 21.75070940071315562, -33.00000000000012790 ) ) ;
#8475 = DIRECTION ( 'NONE',  ( -0.8381289428352193260, -0.5454721580263449665, 0.000000000000000000 ) ) ;
#8476 = ADVANCED_FACE ( 'NONE', ( #8778 ), #9093, .T. ) ;
#8477 = ORIENTED_EDGE ( 'NONE', *, *, #1492, .F. ) ;
#8478 = DIRECTION ( 'NONE',  ( 0.000000000000000000, -1.734723475976817547E-15, 1.000000000000000000 ) ) ;
#8479 = DIRECTION ( 'NONE',  ( 1.000000000000000000, 0.000000000000000000, 0.000000000000000000 ) ) ;
#8480 = FACE_OUTER_BOUND ( 'NONE', #9850, .T. ) ;
#8481 = ORIENTED_EDGE ( 'NONE', *, *, #14855, .T. ) ;
#8482 = CARTESIAN_POINT ( 'NONE',  ( -21.85476584171706449, 5.329050157244580532, 48.50000000000012079 ) ) ;
#8483 = EDGE_CURVE ( 'NONE', #9073, #13749, #14990, .T. ) ;
#8484 = ORIENTED_EDGE ( 'NONE', *, *, #15200, .F. ) ;
#8485 = CARTESIAN_POINT ( 'NONE',  ( 31.72322230991231962, -61.42570632716525125, -2.132522520905369312 ) ) ;
#8486 = LINE ( 'NONE', #12521, #1133 ) ;
#8487 = EDGE_CURVE ( 'NONE', #2597, #1844, #14420, .T. ) ;
#8488 = ORIENTED_EDGE ( 'NONE', *, *, #12870, .F. ) ;
#8489 = APPLICATION_PROTOCOL_DEFINITION ( 'draft international standard', 'automotive_design', 1998, #2443 ) ;
#8490 = FACE_OUTER_BOUND ( 'NONE', #7690, .T. ) ;
#8491 = DIRECTION ( 'NONE',  ( 0.000000000000000000, 1.000000000000000000, -0.000000000000000000 ) ) ;
#8492 = CARTESIAN_POINT ( 'NONE',  ( -8.779681704480811533, 2.489320016922789147, -48.36903577193039894 ) ) ;
#8493 = CARTESIAN_POINT ( 'NONE',  ( 18.00340353969509266, -60.79495753912624423, 6.390225278796973996 ) ) ;
#8494 = CARTESIAN_POINT ( 'NONE',  ( 114.6731053250840233, 23.25070940071369563, 33.00000000000012790 ) ) ;
#8495 = CYLINDRICAL_SURFACE ( 'NONE', #7853, 0.7892041907098262810 ) ;
#8496 = EDGE_CURVE ( 'NONE', #13863, #13766, #1715, .T. ) ;
#8497 = CARTESIAN_POINT ( 'NONE',  ( 33.63218978277217985, -56.84102507669816617, 1.823659438126836285 ) ) ;
#8498 = CARTESIAN_POINT ( 'NONE',  ( 31.56297971567678928, -52.84914412566560316, -3.506280953151710289 ) ) ;
#8499 = EDGE_CURVE ( 'NONE', #12128, #2824, #6883, .T. ) ;
#8500 = DIRECTION ( 'NONE',  ( 0.000000000000000000, 0.000000000000000000, 1.000000000000000000 ) ) ;
#8501 = ORIENTED_EDGE ( 'NONE', *, *, #3944, .F. ) ;
#8502 = DIRECTION ( 'NONE',  ( 0.8208219420614780715, -0.4549890321264283277, -0.3453061251629916950 ) ) ;
#8503 = DIRECTION ( 'NONE',  ( 0.5006040828730228265, -0.8656763553493070917, 0.000000000000000000 ) ) ;
#8504 = CARTESIAN_POINT ( 'NONE',  ( 69.41360828637785119, -3.335076845702578119, 76.94374568549258697 ) ) ;
#8505 = CARTESIAN_POINT ( 'NONE',  ( -20.99999999999998579, -2.249290599286159598, 33.00000000000012790 ) ) ;
#8506 = CARTESIAN_POINT ( 'NONE',  ( 65.67990869784712515, -11.76427225047157776, 72.39415457105613427 ) ) ;
#8507 = CARTESIAN_POINT ( 'NONE',  ( -24.80190064845255193, -6.760980556683136911, 48.50000000000010658 ) ) ;
#8508 = VECTOR ( 'NONE', #4245, 1000.000000000000000 ) ;
#8509 = VERTEX_POINT ( 'NONE', #4160 ) ;
#8510 = DIRECTION ( 'NONE',  ( 0.000000000000000000, 1.000000000000000000, 0.000000000000000000 ) ) ;
#8511 = APPLICATION_CONTEXT ( 'automotive_design' ) ;
#8512 = EDGE_CURVE ( 'NONE', #3697, #404, #13554, .T. ) ;
#8513 = ORIENTED_EDGE ( 'NONE', *, *, #2368, .T. ) ;
#8514 = CARTESIAN_POINT ( 'NONE',  ( 8.599030766203958009, -59.21224831720011395, -1.832439066039622144 ) ) ;
#8515 = ORIENTED_EDGE ( 'NONE', *, *, #1131, .F. ) ;
#8516 = CARTESIAN_POINT ( 'NONE',  ( -10.14179456814604130, -8.352437357651758987, 48.12676452506694602 ) ) ;
#8517 = LINE ( 'NONE', #2667, #13198 ) ;
#8518 = EDGE_CURVE ( 'NONE', #13079, #3246, #250, .T. ) ;
#8519 = CIRCLE ( 'NONE', #10481, 2.524999999999999467 ) ;
#8520 = DIRECTION ( 'NONE',  ( -0.000000000000000000, -0.000000000000000000, -1.000000000000000000 ) ) ;
#8521 = CARTESIAN_POINT ( 'NONE',  ( 8.248019633484567237, -55.36884115291471176, 1.950692953654363127 ) ) ;
#8522 = FACE_OUTER_BOUND ( 'NONE', #14574, .T. ) ;
#8523 = CARTESIAN_POINT ( 'NONE',  ( 76.78650653802468184, -6.946050879336882922, 75.19766410831374515 ) ) ;
#8524 = CIRCLE ( 'NONE', #639, 0.7892041907098262810 ) ;
#8525 = ORIENTED_EDGE ( 'NONE', *, *, #3409, .T. ) ;
#8526 = EDGE_LOOP ( 'NONE', ( #6278, #10537, #2437, #616 ) ) ;
#8527 = AXIS2_PLACEMENT_3D ( 'NONE', #1208, #14898, #12919 ) ;
#8528 = ADVANCED_FACE ( 'NONE', ( #1707 ), #7635, .T. ) ;
#8529 = LINE ( 'NONE', #8380, #11218 ) ;
#8530 = EDGE_CURVE ( 'NONE', #8969, #3666, #2794, .T. ) ;
#8531 = VERTEX_POINT ( 'NONE', #5031 ) ;
#8532 = CARTESIAN_POINT ( 'NONE',  ( -21.85476584171713199, 5.329050157244537900, 48.50000000000012079 ) ) ;
#8533 = VERTEX_POINT ( 'NONE', #1782 ) ;
#8534 = CARTESIAN_POINT ( 'NONE',  ( 16.19211320117534925, -53.25924031079303234, 5.665074923594178635 ) ) ;
#8535 = AXIS2_PLACEMENT_3D ( 'NONE', #2976, #442, #1673 ) ;
#8536 = VERTEX_POINT ( 'NONE', #13397 ) ;
#8537 = CARTESIAN_POINT ( 'NONE',  ( -28.95977857253364007, -8.587818791446682809, 58.00000000000012079 ) ) ;
#8538 = LINE ( 'NONE', #11991, #9443 ) ;
#8539 = ORIENTED_EDGE ( 'NONE', *, *, #5899, .T. ) ;
#8540 = AXIS2_PLACEMENT_3D ( 'NONE', #9929, #14604, #4053 ) ;
#8541 = CARTESIAN_POINT ( 'NONE',  ( 28.71810018070638648, -65.29678988936899486, -3.348867343500047333 ) ) ;
#8542 = CARTESIAN_POINT ( 'NONE',  ( -16.99999999999998579, -2.249290599286303927, -47.50000000000012079 ) ) ;
#8543 = VERTEX_POINT ( 'NONE', #12174 ) ;
#8544 = CARTESIAN_POINT ( 'NONE',  ( 25.18496984658902349, -69.39711819508849544, -5.637959728397561321 ) ) ;
#8545 = DIRECTION ( 'NONE',  ( 1.000000000000000000, 0.000000000000000000, 0.000000000000000000 ) ) ;
#8546 = LINE ( 'NONE', #7392, #8460 ) ;
#8547 = ORIENTED_EDGE ( 'NONE', *, *, #7541, .T. ) ;
#8548 = ADVANCED_FACE ( 'NONE', ( #13263 ), #7348, .F. ) ;
#8549 = ORIENTED_EDGE ( 'NONE', *, *, #3417, .T. ) ;
#8550 = VECTOR ( 'NONE', #12389, 1000.000000000000000 ) ;
#8551 = EDGE_LOOP ( 'NONE', ( #10111, #10637, #8463, #14214 ) ) ;
#8552 = DIRECTION ( 'NONE',  ( -1.000000000000000000, -1.734723475976807292E-15, 0.000000000000000000 ) ) ;
#8553 = ORIENTED_EDGE ( 'NONE', *, *, #10191, .F. ) ;
#8554 = CARTESIAN_POINT ( 'NONE',  ( 62.30678795759143185, -4.906903613034745426, 48.51982618741349285 ) ) ;
#8555 = CARTESIAN_POINT ( 'NONE',  ( -0.9277479332649583021, -2.641590149077306826, 48.50000000000012079 ) ) ;
#8556 = CARTESIAN_POINT ( 'NONE',  ( -8.593267841128518825, 2.185894787177926624, -48.01308457333531265 ) ) ;
#8557 = FACE_OUTER_BOUND ( 'NONE', #8617, .T. ) ;
#8558 = VECTOR ( 'NONE', #11791, 1000.000000000000000 ) ;
#8559 = CARTESIAN_POINT ( 'NONE',  ( 32.05890019364250065, -61.13673569060787827, 2.043233430235019910 ) ) ;
#8560 = LINE ( 'NONE', #398, #7120 ) ;
#8561 = CARTESIAN_POINT ( 'NONE',  ( 104.9938193859979236, 0.000000000000000000, -33.00000000000012790 ) ) ;
#8562 = CARTESIAN_POINT ( 'NONE',  ( 31.87807348626150983, -54.14081474687885276, -3.331943113775099441 ) ) ;
#8563 = CARTESIAN_POINT ( 'NONE',  ( 27.55953187330915810, 0.000000000000000000, 139.1143251403882459 ) ) ;
#8564 = VERTEX_POINT ( 'NONE', #4306 ) ;
#8565 = CARTESIAN_POINT ( 'NONE',  ( 42.07846078193830408, 23.25070940071368852, 139.1143251403882459 ) ) ;
#8566 = LINE ( 'NONE', #3938, #2941 ) ;
#8567 = DIRECTION ( 'NONE',  ( 0.000000000000000000, 0.000000000000000000, 1.000000000000000000 ) ) ;
#8568 = DIRECTION ( 'NONE',  ( 0.9111637130653279515, 0.4120445218577777902, 0.000000000000000000 ) ) ;
#8569 = ADVANCED_FACE ( 'NONE', ( #9011 ), #14783, .F. ) ;
#8570 = EDGE_CURVE ( 'NONE', #538, #14822, #4236, .T. ) ;
#8571 = CARTESIAN_POINT ( 'NONE',  ( 69.45041322604760126, -2.827919977413038133, 76.54331634761751957 ) ) ;
#8572 = EDGE_CURVE ( 'NONE', #14721, #5437, #847, .T. ) ;
#8573 = CARTESIAN_POINT ( 'NONE',  ( 29.35555050496135721, -53.24929059928630437, -3.199931146564412021 ) ) ;
#8574 = FACE_OUTER_BOUND ( 'NONE', #5088, .T. ) ;
#8575 = ADVANCED_FACE ( 'NONE', ( #3164 ), #6852, .T. ) ;
#8576 = FACE_OUTER_BOUND ( 'NONE', #11650, .T. ) ;
#8577 = EDGE_LOOP ( 'NONE', ( #10158, #7633, #9840, #6642 ) ) ;
#8578 = FACE_OUTER_BOUND ( 'NONE', #13560, .T. ) ;
#8579 = UNCERTAINTY_MEASURE_WITH_UNIT (LENGTH_MEASURE( 1.000000000000000082E-05 ), #854, 'distance_accuracy_value', 'NONE');
#8580 = ORIENTED_EDGE ( 'NONE', *, *, #14888, .T. ) ;
#8581 = DIRECTION ( 'NONE',  ( -0.000000000000000000, -1.000000000000000000, -1.734723475976817547E-15 ) ) ;
#8582 = FACE_OUTER_BOUND ( 'NONE', #4792, .T. ) ;
#8583 = VERTEX_POINT ( 'NONE', #6544 ) ;
#8584 = DIRECTION ( 'NONE',  ( -1.000000000000000000, -0.000000000000000000, -0.000000000000000000 ) ) ;
#8585 = DIRECTION ( 'NONE',  ( -0.000000000000000000, -0.000000000000000000, 1.000000000000000000 ) ) ;
#8586 = TOROIDAL_SURFACE ( 'NONE', #10561, 7.924024642120688355, 1.000000000000000000 ) ;
#8587 = AXIS2_PLACEMENT_3D ( 'NONE', #12480, #7946, #2165 ) ;
#8588 = FACE_OUTER_BOUND ( 'NONE', #10457, .T. ) ;
#8589 = DIRECTION ( 'NONE',  ( 0.000000000000000000, 1.000000000000000000, 0.000000000000000000 ) ) ;
#8590 = ADVANCED_FACE ( 'NONE', ( #5635 ), #4167, .T. ) ;
#8591 = DIRECTION ( 'NONE',  ( 0.000000000000000000, 0.000000000000000000, 1.000000000000000000 ) ) ;
#8592 = CARTESIAN_POINT ( 'NONE',  ( 118.0000000000000284, 23.25070940071369563, -33.00000000000012790 ) ) ;
#8593 = AXIS2_PLACEMENT_3D ( 'NONE', #11597, #3212, #6905 ) ;
#8594 = AXIS2_PLACEMENT_3D ( 'NONE', #185, #10578, #6039 ) ;
#8595 = ORIENTED_EDGE ( 'NONE', *, *, #7333, .T. ) ;
#8596 = EDGE_LOOP ( 'NONE', ( #13225, #1354, #11012, #11705 ) ) ;
#8597 = FACE_OUTER_BOUND ( 'NONE', #10153, .T. ) ;
#8598 = EDGE_LOOP ( 'NONE', ( #6615, #373, #7079, #4566 ) ) ;
#8599 = CARTESIAN_POINT ( 'NONE',  ( 114.0000000000000284, 15.25070940071369563, 13.14990448602693007 ) ) ;
#8600 = ORIENTED_EDGE ( 'NONE', *, *, #4333, .T. ) ;
#8601 = CARTESIAN_POINT ( 'NONE',  ( 29.05371116072213056, -64.60713873539394569, 3.212402267255086930 ) ) ;
#8602 = ORIENTED_EDGE ( 'NONE', *, *, #13924, .F. ) ;
#8603 = DIRECTION ( 'NONE',  ( 0.000000000000000000, -1.000000000000000000, 0.000000000000000000 ) ) ;
#8604 = FACE_OUTER_BOUND ( 'NONE', #1289, .T. ) ;
#8605 = ORIENTED_EDGE ( 'NONE', *, *, #8411, .F. ) ;
#8606 = AXIS2_PLACEMENT_3D ( 'NONE', #11987, #8385, #7148 ) ;
#8607 = CARTESIAN_POINT ( 'NONE',  ( 28.31271169503250107, -66.37912134691313781, -3.509717431437875845 ) ) ;
#8608 = ORIENTED_EDGE ( 'NONE', *, *, #13520, .F. ) ;
#8609 = EDGE_CURVE ( 'NONE', #11451, #10712, #9178, .T. ) ;
#8610 = EDGE_CURVE ( 'NONE', #10346, #1708, #10246, .T. ) ;
#8611 = DIRECTION ( 'NONE',  ( 0.8746197071345573892, -0.4848096202550657430, 0.000000000000000000 ) ) ;
#8612 = CARTESIAN_POINT ( 'NONE',  ( 62.88869237673507229, 0.3854521819929429549, 48.51982618741349285 ) ) ;
#8613 = LINE ( 'NONE', #12083, #7953 ) ;
#8614 = ORIENTED_EDGE ( 'NONE', *, *, #5413, .T. ) ;
#8615 = CARTESIAN_POINT ( 'NONE',  ( -23.68178719075091365, 3.790042057515504048, 47.74919337097016836 ) ) ;
#8616 = ORIENTED_EDGE ( 'NONE', *, *, #7456, .F. ) ;
#8617 = EDGE_LOOP ( 'NONE', ( #418, #5851, #3472, #9156, #14957, #10306, #14141 ) ) ;
#8618 = DIRECTION ( 'NONE',  ( 0.000000000000000000, 0.000000000000000000, -1.000000000000000000 ) ) ;
#8619 = VERTEX_POINT ( 'NONE', #4549 ) ;
#8620 = APPLICATION_PROTOCOL_DEFINITION ( 'draft international standard', 'automotive_design', 1998, #8324 ) ;
#8621 = CARTESIAN_POINT ( 'NONE',  ( 72.26742264675378635, -14.73126838498887281, 76.19766410831374515 ) ) ;
#8622 = CARTESIAN_POINT ( 'NONE',  ( -16.99999999999998579, -6.754727345143736628, 36.00000000000012079 ) ) ;
#8623 = EDGE_CURVE ( 'NONE', #3925, #13020, #2084, .T. ) ;
#8624 = CARTESIAN_POINT ( 'NONE',  ( 23.36173033120691400, -82.24929059928629727, 6.000000000000001776 ) ) ;
#8625 = AXIS2_PLACEMENT_3D ( 'NONE', #5516, #9207, #14972 ) ;
#8626 = EDGE_CURVE ( 'NONE', #6859, #11898, #15018, .T. ) ;
#8627 = CARTESIAN_POINT ( 'NONE',  ( 17.70648456744905275, -67.68160391992790892, 6.249260988556712526 ) ) ;
#8628 = CARTESIAN_POINT ( 'NONE',  ( -8.787473001628837821, 2.499856724289235554, -48.50000000000012079 ) ) ;
#8629 = CARTESIAN_POINT ( 'NONE',  ( 69.46454297106444642, -2.294433322023680333, 75.19766410831374515 ) ) ;
#8630 = DIRECTION ( 'NONE',  ( 1.000000000000000000, -3.565820478396769525E-15, 0.000000000000000000 ) ) ;
#8631 = CARTESIAN_POINT ( 'NONE',  ( 32.44598258732901286, -53.56578013995665088, -2.318572182806100557 ) ) ;
#8632 = VECTOR ( 'NONE', #1709, 1000.000000000000000 ) ;
#8633 = DIRECTION ( 'NONE',  ( 0.000000000000000000, 1.000000000000000000, 0.000000000000000000 ) ) ;
#8634 = ORIENTED_EDGE ( 'NONE', *, *, #14956, .F. ) ;
#8635 = DIRECTION ( 'NONE',  ( 1.000000000000000000, 0.000000000000000000, 0.000000000000000000 ) ) ;
#8636 = DIRECTION ( 'NONE',  ( -0.000000000000000000, 1.000000000000000000, -0.000000000000000000 ) ) ;
#8637 = DIRECTION ( 'NONE',  ( 0.000000000000000000, 0.000000000000000000, -1.000000000000000000 ) ) ;
#8638 = CARTESIAN_POINT ( 'NONE',  ( 63.03271294676726910, -4.597264848142476268, 54.56811043785582882 ) ) ;
#8639 = VECTOR ( 'NONE', #620, 1000.000000000000000 ) ;
#8640 = CARTESIAN_POINT ( 'NONE',  ( 64.68848588106907016, -11.56114324328357057, 71.69770485003853366 ) ) ;
#8641 = VECTOR ( 'NONE', #2611, 1000.000000000000000 ) ;
#8642 = PRESENTATION_LAYER_ASSIGNMENT (  '', '', ( #533 ) ) ;
#8643 = EDGE_CURVE ( 'NONE', #251, #4675, #9094, .T. ) ;
#8644 = CARTESIAN_POINT ( 'NONE',  ( 108.0866310645538562, 21.75070940071366365, 139.1143251403882459 ) ) ;
#8645 = LINE ( 'NONE', #11755, #10366 ) ;
#8646 = EDGE_CURVE ( 'NONE', #1117, #2307, #6775, .T. ) ;
#8647 = ORIENTED_EDGE ( 'NONE', *, *, #157, .T. ) ;
#8648 = ADVANCED_FACE ( 'NONE', ( #13862 ), #13781, .T. ) ;
#8649 = CARTESIAN_POINT ( 'NONE',  ( 32.22797764705516244, -60.90019506145032580, -2.720530867584999513 ) ) ;
#8650 = PRESENTATION_LAYER_ASSIGNMENT (  '', '', ( #12580 ) ) ;
#8651 = AXIS2_PLACEMENT_3D ( 'NONE', #5695, #5778, #14000 ) ;
#8652 = VERTEX_POINT ( 'NONE', #7943 ) ;
#8653 = LINE ( 'NONE', #7575, #10117 ) ;
#8654 = CARTESIAN_POINT ( 'NONE',  ( 80.18290120114222930, 25.52935533987996664, 33.00000000000014211 ) ) ;
#8655 = VECTOR ( 'NONE', #7792, 1000.000000000000000 ) ;
#8656 = ORIENTED_EDGE ( 'NONE', *, *, #14758, .F. ) ;
#8657 = LINE ( 'NONE', #2814, #10643 ) ;
#8658 = DIRECTION ( 'NONE',  ( 0.000000000000000000, 0.000000000000000000, -1.000000000000000000 ) ) ;
#8659 = ADVANCED_FACE ( 'NONE', ( #9465 ), #4090, .T. ) ;
#8660 = ADVANCED_FACE ( 'NONE', ( #303 ), #7298, .T. ) ;
#8661 = DIRECTION ( 'NONE',  ( -1.000000000000000000, 0.000000000000000000, 0.000000000000000000 ) ) ;
#8662 = ORIENTED_EDGE ( 'NONE', *, *, #3917, .F. ) ;
#8663 = AXIS2_PLACEMENT_3D ( 'NONE', #7359, #9968, #5195 ) ;
#8664 = CARTESIAN_POINT ( 'NONE',  ( 10.86504213735824642, -53.50006564588471036, 3.720697674322940962 ) ) ;
#8665 = DIRECTION ( 'NONE',  ( -1.000000000000000000, 0.000000000000000000, 0.000000000000000000 ) ) ;
#8666 = DIRECTION ( 'NONE',  ( -0.000000000000000000, -0.000000000000000000, -1.000000000000000000 ) ) ;
#8667 = VECTOR ( 'NONE', #11593, 1000.000000000000000 ) ;
#8668 = EDGE_CURVE ( 'NONE', #143, #10195, #10408, .T. ) ;
#8669 = EDGE_LOOP ( 'NONE', ( #7051, #10385, #4899, #4531 ) ) ;
#8670 = EDGE_CURVE ( 'NONE', #7200, #3379, #2713, .T. ) ;
#8671 = EDGE_LOOP ( 'NONE', ( #5519, #10673, #8602, #11585 ) ) ;
#8672 = DIRECTION ( 'NONE',  ( -0.000000000000000000, 0.000000000000000000, -1.000000000000000000 ) ) ;
#8673 = ORIENTED_EDGE ( 'NONE', *, *, #8934, .T. ) ;
#8674 = FACE_OUTER_BOUND ( 'NONE', #7581, .T. ) ;
#8675 = ORIENTED_EDGE ( 'NONE', *, *, #11630, .T. ) ;
#8676 = AXIS2_PLACEMENT_3D ( 'NONE', #5300, #14679, #8830 ) ;
#8677 = ADVANCED_BREP_SHAPE_REPRESENTATION ( '', ( #14200, #6315 ), #4840 ) ;
#8678 = DIRECTION ( 'NONE',  ( 0.8208219420614786266, -0.4549890321264269399, -0.3453061251629920836 ) ) ;
#8679 = CARTESIAN_POINT ( 'NONE',  ( -26.99999999999998934, -2.249290599286303927, 33.00000000000012790 ) ) ;
#8680 = EDGE_LOOP ( 'NONE', ( #10441, #807, #11602, #5263 ) ) ;
#8681 = AXIS2_PLACEMENT_3D ( 'NONE', #10705, #162, #9561 ) ;
#8682 = CARTESIAN_POINT ( 'NONE',  ( -9.037775043065352065, 2.932694901963889489, -57.50000000000012079 ) ) ;
#8683 = ORIENTED_EDGE ( 'NONE', *, *, #5426, .T. ) ;
#8684 = DIRECTION ( 'NONE',  ( 1.156482317317870492E-16, -1.000000000000000000, 0.000000000000000000 ) ) ;
#8685 = FACE_OUTER_BOUND ( 'NONE', #1743, .T. ) ;
#8686 = FACE_OUTER_BOUND ( 'NONE', #2024, .T. ) ;
#8687 = EDGE_LOOP ( 'NONE', ( #15141, #13635, #11162 ) ) ;
#8688 = DIRECTION ( 'NONE',  ( 1.239088197126290570E-16, -1.000000000000000000, -1.734723475976817744E-15 ) ) ;
#8689 = EDGE_LOOP ( 'NONE', ( #2699, #12303, #12834, #7414 ) ) ;
#8690 = VECTOR ( 'NONE', #4435, 1000.000000000000000 ) ;
#8691 = ORIENTED_EDGE ( 'NONE', *, *, #3189, .F. ) ;
#8692 = VERTEX_POINT ( 'NONE', #2536 ) ;
#8693 = ADVANCED_FACE ( 'NONE', ( #1295 ), #7630, .T. ) ;
#8694 = LINE ( 'NONE', #7397, #14311 ) ;
#8695 = CONTEXT_DEPENDENT_SHAPE_REPRESENTATION ( #12662, #5074 ) ;
#8696 = DIRECTION ( 'NONE',  ( 0.000000000000000000, 0.000000000000000000, 1.000000000000000000 ) ) ;
#8697 = LINE ( 'NONE', #7401, #14802 ) ;
#8698 = LINE ( 'NONE', #10950, #14632 ) ;
#8699 = VERTEX_POINT ( 'NONE', #4995 ) ;
#8700 = CARTESIAN_POINT ( 'NONE',  ( 12.93430674223484012, -54.56989982945474793, 4.214561586068453991 ) ) ;
#8701 = CARTESIAN_POINT ( 'NONE',  ( 40.00000000000002132, 23.95881716715919652, 33.00000000000017053 ) ) ;
#8702 = CARTESIAN_POINT ( 'NONE',  ( 65.00000000000001421, -85.24929059928631148, 19.99999999999999645 ) ) ;
#8703 = DIRECTION ( 'NONE',  ( 0.000000000000000000, 0.000000000000000000, -1.000000000000000000 ) ) ;
#8704 = CARTESIAN_POINT ( 'NONE',  ( 13.49335920019348833, -64.93526722763056114, -4.251815205945797871 ) ) ;
#8705 = DIRECTION ( 'NONE',  ( -0.000000000000000000, 0.000000000000000000, 1.000000000000000000 ) ) ;
#8706 = EDGE_CURVE ( 'NONE', #1096, #3386, #148, .T. ) ;
#8707 = ORIENTED_EDGE ( 'NONE', *, *, #1222, .F. ) ;
#8708 = FACE_OUTER_BOUND ( 'NONE', #13358, .T. ) ;
#8709 = DIRECTION ( 'NONE',  ( -0.2245716668862471899, -0.9744202983869689749, -0.008523410314122886050 ) ) ;
#8710 =( LENGTH_UNIT ( ) NAMED_UNIT ( * ) SI_UNIT ( .MILLI., .METRE. ) );
#8711 = DIRECTION ( 'NONE',  ( -0.000000000000000000, 0.000000000000000000, 1.000000000000000000 ) ) ;
#8712 = CARTESIAN_POINT ( 'NONE',  ( 10.85656041602113753, -53.50334687180571791, 3.717581709362825393 ) ) ;
#8713 = DIRECTION ( 'NONE',  ( 0.000000000000000000, 1.000000000000000000, 1.734723475976817744E-15 ) ) ;
#8714 = CARTESIAN_POINT ( 'NONE',  ( -80.00000000000001421, -85.24929059928629727, 8.000000000000001776 ) ) ;
#8715 = CARTESIAN_POINT ( 'NONE',  ( 29.66000553811799634, -63.57773214734891098, -2.964070158660720100 ) ) ;
#8716 = APPLICATION_CONTEXT ( 'automotive_design' ) ;
#8717 = ORIENTED_EDGE ( 'NONE', *, *, #1309, .F. ) ;
#8718 = CARTESIAN_POINT ( 'NONE',  ( 28.85714878300505504, -53.69100233675187894, -4.215531945130809532 ) ) ;
#8719 = ORIENTED_EDGE ( 'NONE', *, *, #4076, .T. ) ;
#8720 = LINE ( 'NONE', #14645, #4719 ) ;
#8721 = DIRECTION ( 'NONE',  ( 0.000000000000000000, -0.000000000000000000, 1.000000000000000000 ) ) ;
#8722 = ORIENTED_EDGE ( 'NONE', *, *, #13610, .T. ) ;
#8723 = DIRECTION ( 'NONE',  ( -0.000000000000000000, 1.445602896647339163E-16, 1.000000000000000000 ) ) ;
#8724 = CARTESIAN_POINT ( 'NONE',  ( 9.200644618036294631, -59.06479067038043240, 2.757123406423048984 ) ) ;
#8725 = B_SPLINE_CURVE_WITH_KNOTS ( 'NONE', 3,
 ( #14896, #10444, #11669, #1116, #9291, #5833, #15065, #6740, #4352, #10293, #14982, #4513, #2208, #9217 ),
 .UNSPECIFIED., .F., .F.,
 ( 4, 2, 2, 2, 2, 2, 4 ),
 ( 5.333844516275199261E-16, 0.002515995007885866910, 0.003773992511828533000, 0.005031990015771198657, 0.006289987519713865181, 0.007547985023656532573, 0.01006398003154186128 ),
 .UNSPECIFIED. ) ;
#8726 = B_SPLINE_CURVE_WITH_KNOTS ( 'NONE', 3,
 ( #4820, #9523, #10745, #15135 ),
 .UNSPECIFIED., .F., .F.,
 ( 4, 4 ),
 ( 0.000000000000000000, 0.001771943201165731424 ),
 .UNSPECIFIED. ) ;
#8727 = DIRECTION ( 'NONE',  ( -0.7546336727145995793, -0.5961293309129263029, -0.2741493039031495660 ) ) ;
#8728 = VECTOR ( 'NONE', #5729, 1000.000000000000000 ) ;
#8729 = CARTESIAN_POINT ( 'NONE',  ( 9.783312177552611288, -53.10528739703777745, 3.364210193422589423 ) ) ;
#8730 = DIRECTION ( 'NONE',  ( 6.938893903907228378E-17, 1.000000000000000000, -0.000000000000000000 ) ) ;
#8731 = CARTESIAN_POINT ( 'NONE',  ( 47.97280705105441001, 3.308873213108444400, 81.40005259842790508 ) ) ;
#8732 = EDGE_CURVE ( 'NONE', #3976, #6117, #11803, .T. ) ;
#8733 = ORIENTED_EDGE ( 'NONE', *, *, #1829, .F. ) ;
#8734 = ORIENTED_EDGE ( 'NONE', *, *, #11279, .F. ) ;
#8735 = CARTESIAN_POINT ( 'NONE',  ( -12.33418063572647938, -2.249290599286303927, -57.50000000000012079 ) ) ;
#8736 = VERTEX_POINT ( 'NONE', #9846 ) ;
#8737 = ORIENTED_EDGE ( 'NONE', *, *, #12289, .F. ) ;
#8738 = CARTESIAN_POINT ( 'NONE',  ( 30.63598825987613949, -53.42215338339671149, -3.801984355195810128 ) ) ;
#8739 = ORIENTED_EDGE ( 'NONE', *, *, #13638, .F. ) ;
#8740 = CARTESIAN_POINT ( 'NONE',  ( 58.00000000000000711, -2.249290599286309256, 82.40005259842790508 ) ) ;
#8741 = CARTESIAN_POINT ( 'NONE',  ( 80.18290120114222930, 29.52935533987996664, -21.00807340887166674 ) ) ;
#8742 = ORIENTED_EDGE ( 'NONE', *, *, #14496, .T. ) ;
#8743 = CARTESIAN_POINT ( 'NONE',  ( -9.037775043065352065, 2.932694901963889489, 57.50000000000012079 ) ) ;
#8744 = CARTESIAN_POINT ( 'NONE',  ( 56.25419740419757630, 3.022649838004307199, 60.61639468829817190 ) ) ;
#8745 = ORIENTED_EDGE ( 'NONE', *, *, #4166, .F. ) ;
#8746 = ADVANCED_FACE ( 'NONE', ( #9622 ), #12464, .T. ) ;
#8747 = EDGE_CURVE ( 'NONE', #2925, #211, #12045, .T. ) ;
#8748 = CARTESIAN_POINT ( 'NONE',  ( 29.96883933646627440, -63.18892729117106200, -3.546101824481814990 ) ) ;
#8749 = ORIENTED_EDGE ( 'NONE', *, *, #9741, .F. ) ;
#8750 = VECTOR ( 'NONE', #4614, 1000.000000000000000 ) ;
#8751 = AXIS2_PLACEMENT_3D ( 'NONE', #15215, #10527, #9293 ) ;
#8752 = FACE_OUTER_BOUND ( 'NONE', #2774, .T. ) ;
#8753 = LINE ( 'NONE', #13451, #6186 ) ;
#8754 = DIRECTION ( 'NONE',  ( -0.000000000000000000, -0.000000000000000000, -1.000000000000000000 ) ) ;
#8755 = FACE_OUTER_BOUND ( 'NONE', #8429, .T. ) ;
#8756 = EDGE_LOOP ( 'NONE', ( #443, #9563, #5337, #2163 ) ) ;
#8757 = DIRECTION ( 'NONE',  ( 0.000000000000000000, 0.000000000000000000, 1.000000000000000000 ) ) ;
#8758 = AXIS2_PLACEMENT_3D ( 'NONE', #14739, #5360, #11662 ) ;
#8759 = ORIENTED_EDGE ( 'NONE', *, *, #6126, .T. ) ;
#8760 = VERTEX_POINT ( 'NONE', #3975 ) ;
#8761 =( LENGTH_UNIT ( ) NAMED_UNIT ( * ) SI_UNIT ( .MILLI., .METRE. ) );
#8762 = AXIS2_PLACEMENT_3D ( 'NONE', #12603, #14746, #2053 ) ;
#8763 = AXIS2_PLACEMENT_3D ( 'NONE', #3658, #14274, #7340 ) ;
#8764 = CARTESIAN_POINT ( 'NONE',  ( 73.69809405469877106, 25.52935533987996664, 21.00807340887166674 ) ) ;
#8765 = DIRECTION ( 'NONE',  ( 0.000000000000000000, -1.000000000000000000, 0.000000000000000000 ) ) ;
#8766 = DIRECTION ( 'NONE',  ( 0.000000000000000000, 0.000000000000000000, 1.000000000000000000 ) ) ;
#8767 = VERTEX_POINT ( 'NONE', #1678 ) ;
#8768 = VECTOR ( 'NONE', #1287, 1000.000000000000000 ) ;
#8769 = CARTESIAN_POINT ( 'NONE',  ( 70.17742216864051841, -3.884085244343386645, 76.08660377794682006 ) ) ;
#8770 = CARTESIAN_POINT ( 'NONE',  ( 61.93276294469178822, -4.429256696798314685, 86.40005259842790508 ) ) ;
#8771 = VECTOR ( 'NONE', #13855, 1000.000000000000000 ) ;
#8772 = EDGE_CURVE ( 'NONE', #2535, #7467, #7831, .T. ) ;
#8773 = CYLINDRICAL_SURFACE ( 'NONE', #7686, 9.000000000000001776 ) ;
#8774 = CARTESIAN_POINT ( 'NONE',  ( 11.00886140161535387, -62.29356353673586000, -3.270869388470717176 ) ) ;
#8775 = ORIENTED_EDGE ( 'NONE', *, *, #9435, .F. ) ;
#8776 = AXIS2_PLACEMENT_3D ( 'NONE', #4145, #1767, #5239 ) ;
#8777 = CARTESIAN_POINT ( 'NONE',  ( 118.0000000000000284, 23.25070940071369563, -13.14990448602692474 ) ) ;
#8778 = FACE_OUTER_BOUND ( 'NONE', #8756, .T. ) ;
#8779 = VERTEX_POINT ( 'NONE', #657 ) ;
#8780 = FILL_AREA_STYLE ('',( #4080 ) ) ;
#8781 = CARTESIAN_POINT ( 'NONE',  ( 62.70356846721307420, -0.3817325368051065482, 60.61639468829817190 ) ) ;
#8782 = CIRCLE ( 'NONE', #1422, 3.000000000000002665 ) ;
#8783 = DIRECTION ( 'NONE',  ( -0.5006040828730242698, 0.8656763553493063146, 0.000000000000000000 ) ) ;
#8784 = DIRECTION ( 'NONE',  ( 0.8746197071345503948, -0.4848096202550782885, 0.000000000000000000 ) ) ;
#8785 = ORIENTED_EDGE ( 'NONE', *, *, #10082, .T. ) ;
#8786 = CLOSED_SHELL ( 'NONE', ( #6832, #9942, #14353, #10896, #7628, #9801, #8305, #13222, #12515, #7014, #3945, #140, #11474, #1783, #8111, #4762, #6768, #9973, #9857, #610, #3169, #14987, #12932, #1610, #9099, #2650, #3855, #14404, #3168, #10473, #27, #11566, #14334, #6177, #2599, #3211, #10263, #3050, #9583, #10314, #3863, #13274, #5019, #5285, #12660, #15023, #4075, #3351, #3878, #692, #5185, #13396, #4907, #3362, #10941, #4544, #12644, #1971, #11953, #13216, #5243, #13154, #11737, #6198, #2107, #14589, #3941, #3777, #2832, #11278, #11567, #1461, #10975, #10639, #8872, #2915, #10839, #6106, #4144, #7210, #14715, #6576, #6470, #12139, #7211, #6622, #2271, #5763, #7084, #3394, #10882, #11821 ) ) ;
#8787 = CIRCLE ( 'NONE', #9298, 3.694885682587998765 ) ;
#8788 = AXIS2_PLACEMENT_3D ( 'NONE', #7462, #12149, #10995 ) ;
#8789 = CARTESIAN_POINT ( 'NONE',  ( -3.190546569013415379, 0.8906624217387615339, 57.50000000000012079 ) ) ;
#8790 = ADVANCED_FACE ( 'NONE', ( #11133 ), #4044, .T. ) ;
#8791 = CARTESIAN_POINT ( 'NONE',  ( -65.00000000000001421, -85.24929059928629727, -17.47499999999999787 ) ) ;
#8792 = ADVANCED_FACE ( 'NONE', ( #9918 ), #8974, .F. ) ;
#8793 = CARTESIAN_POINT ( 'NONE',  ( -32.80254285330622110, -2.278009980413880697, -48.00000000000012079 ) ) ;
#8794 = LINE ( 'NONE', #13491, #1754 ) ;
#8795 = VECTOR ( 'NONE', #14997, 1000.000000000000000 ) ;
#8796 = ORIENTED_EDGE ( 'NONE', *, *, #11092, .T. ) ;
#8797 = CARTESIAN_POINT ( 'NONE',  ( 23.53111059739647715, -55.08889408819338485, -6.471126372657454162 ) ) ;
#8798 = VERTEX_POINT ( 'NONE', #812 ) ;
#8799 = DIRECTION ( 'NONE',  ( -0.8420378618367675427, -0.5394184268574490071, -0.000000000000000000 ) ) ;
#8800 = CARTESIAN_POINT ( 'NONE',  ( -16.99999999999998579, -2.249290599286303927, 38.50000000000012790 ) ) ;
#8801 = ORIENTED_EDGE ( 'NONE', *, *, #14768, .T. ) ;
#8803 = ORIENTED_EDGE ( 'NONE', *, *, #1872, .F. ) ;
#8802 = DIRECTION ( 'NONE',  ( 1.000000000000000000, 0.000000000000000000, -0.000000000000000000 ) ) ;
#8804 = DIRECTION ( 'NONE',  ( 0.000000000000000000, 1.445602896647339410E-16, -1.000000000000000000 ) ) ;
#8805 = ORIENTED_EDGE ( 'NONE', *, *, #12012, .F. ) ;
#8806 = CARTESIAN_POINT ( 'NONE',  ( 10.59452993935293641, -61.89517205450620452, 2.369674354353247914 ) ) ;
#8807 = EDGE_CURVE ( 'NONE', #11185, #10484, #14737, .T. ) ;
#8808 = CARTESIAN_POINT ( 'NONE',  ( 65.00000000000001421, -85.24929059928631148, 19.99999999999999645 ) ) ;
#8809 = CIRCLE ( 'NONE', #5630, 3.999999999999999112 ) ;
#8810 = PLANE ( 'NONE',  #11138 ) ;
#8811 = CARTESIAN_POINT ( 'NONE',  ( 19.97461805067967688, -85.24929059928631148, -6.000000000000000888 ) ) ;
#8812 = ORIENTED_EDGE ( 'NONE', *, *, #3318, .T. ) ;
#8813 = CARTESIAN_POINT ( 'NONE',  ( 9.754844199345544808, -60.26934622950999199, 2.884867303495438851 ) ) ;
#8814 = ORIENTED_EDGE ( 'NONE', *, *, #6928, .T. ) ;
#8815 = ORIENTED_EDGE ( 'NONE', *, *, #4559, .T. ) ;
#8816 = AXIS2_PLACEMENT_3D ( 'NONE', #3175, #7875, #12567 ) ;
#8817 = DIRECTION ( 'NONE',  ( 0.000000000000000000, 0.000000000000000000, 1.000000000000000000 ) ) ;
#8818 = AXIS2_PLACEMENT_3D ( 'NONE', #10651, #12809, #12647 ) ;
#8819 = ORIENTED_EDGE ( 'NONE', *, *, #12258, .F. ) ;
#8820 = DIRECTION ( 'NONE',  ( 0.3020115420618247892, -0.1674077314120183957, 0.9384901064608620613 ) ) ;
#8821 = CARTESIAN_POINT ( 'NONE',  ( 69.46373988936370836, -2.401367963164388719, 72.55353403238311216 ) ) ;
#8822 = DIRECTION ( 'NONE',  ( -0.8746197071345570562, 0.4848096202550665756, 0.000000000000000000 ) ) ;
#8823 = CARTESIAN_POINT ( 'NONE',  ( 53.27389963060701916, 0.6670697996139958175, 48.51982618741349285 ) ) ;
#8824 = EDGE_LOOP ( 'NONE', ( #13773, #7454, #34, #3418 ) ) ;
#8825 = CARTESIAN_POINT ( 'NONE',  ( 31.49298359385885249, -60.71197230342421136, -3.050751728647392191 ) ) ;
#8826 = VERTEX_POINT ( 'NONE', #5365 ) ;
#8827 = VECTOR ( 'NONE', #1058, 1000.000000000000000 ) ;
#8828 = VECTOR ( 'NONE', #9879, 1000.000000000000000 ) ;
#8829 = DIRECTION ( 'NONE',  ( -1.000000000000000000, 0.000000000000000000, 0.000000000000000000 ) ) ;
#8830 = DIRECTION ( 'NONE',  ( -1.000000000000000000, 0.000000000000000000, 0.000000000000000000 ) ) ;
#8831 = EDGE_CURVE ( 'NONE', #12681, #8031, #1725, .T. ) ;
#8832 = LINE ( 'NONE', #13453, #12362 ) ;
#8833 = ORIENTED_EDGE ( 'NONE', *, *, #4799, .T. ) ;
#8834 = FACE_OUTER_BOUND ( 'NONE', #4547, .T. ) ;
#8835 = ADVANCED_FACE ( 'NONE', ( #7598 ), #12211, .T. ) ;
#8836 = EDGE_LOOP ( 'NONE', ( #2096, #4284, #14940, #12346 ) ) ;
#8837 = ORIENTED_EDGE ( 'NONE', *, *, #3399, .T. ) ;
#8838 = ADVANCED_FACE ( 'NONE', ( #12287 ), #9984, .F. ) ;
#8839 = ADVANCED_FACE ( 'NONE', ( #8674 ), #2982, .F. ) ;
#8840 = ORIENTED_EDGE ( 'NONE', *, *, #3608, .T. ) ;
#8841 = LINE ( 'NONE', #1765, #318 ) ;
#8842 =( GEOMETRIC_REPRESENTATION_CONTEXT ( 3 ) GLOBAL_UNCERTAINTY_ASSIGNED_CONTEXT ( ( #5045 ) ) GLOBAL_UNIT_ASSIGNED_CONTEXT ( ( #13903, #8058, #2955 ) ) REPRESENTATION_CONTEXT ( 'NONE', 'WORKASPACE' ) );
#8843 = ITEM_DEFINED_TRANSFORMATION ( 'NONE', 'NONE', #13689,  #6315 ) ;
#8844 = DIRECTION ( 'NONE',  ( 0.000000000000000000, 0.000000000000000000, 1.000000000000000000 ) ) ;
#8845 = CARTESIAN_POINT ( 'NONE',  ( 80.00000000000001421, -74.24929059928631148, 32.99999999999999289 ) ) ;
#8846 = EDGE_CURVE ( 'NONE', #3165, #6912, #12435, .T. ) ;
#8847 = CARTESIAN_POINT ( 'NONE',  ( -11.58528623411511305, -9.440246857018177451, -48.26816462195812818 ) ) ;
#8848 = ORIENTED_EDGE ( 'NONE', *, *, #5611, .F. ) ;
#8849 = VERTEX_POINT ( 'NONE', #12519 ) ;
#8850 = DIRECTION ( 'NONE',  ( 1.000000000000000000, 0.000000000000000000, -0.000000000000000000 ) ) ;
#8851 = CARTESIAN_POINT ( 'NONE',  ( 33.52366768382369600, -57.47994873761393109, -2.501453769636598601 ) ) ;
#8852 = DIRECTION ( 'NONE',  ( 0.000000000000000000, 0.000000000000000000, 1.000000000000000000 ) ) ;
#8853 = CIRCLE ( 'NONE', #6164, 5.165819364273509073 ) ;
#8854 = LINE ( 'NONE', #14559, #4910 ) ;
#8855 = ORIENTED_EDGE ( 'NONE', *, *, #5121, .F. ) ;
#8856 = CARTESIAN_POINT ( 'NONE',  ( -7.999999999999986677, -2.249290599286302594, 38.50000000000012790 ) ) ;
#8857 = EDGE_CURVE ( 'NONE', #15020, #7147, #1485, .T. ) ;
#8858 = DIRECTION ( 'NONE',  ( -1.000000000000000000, -8.673617379884035472E-17, 0.000000000000000000 ) ) ;
#8859 = ORIENTED_EDGE ( 'NONE', *, *, #3828, .F. ) ;
#8860 = CARTESIAN_POINT ( 'NONE',  ( 47.27423575335444639, 25.52935533987996664, 33.00000000000014211 ) ) ;
#8861 = DIRECTION ( 'NONE',  ( 8.673617379884035472E-17, -1.000000000000000000, 0.000000000000000000 ) ) ;
#8862 = VECTOR ( 'NONE', #12664, 1000.000000000000000 ) ;
#8863 = CARTESIAN_POINT ( 'NONE',  ( -16.99999999999998579, -2.249290599286303927, 38.50000000000012790 ) ) ;
#8864 = ORIENTED_EDGE ( 'NONE', *, *, #14702, .F. ) ;
#8865 = LINE ( 'NONE', #13561, #13905 ) ;
#8866 = AXIS2_PLACEMENT_3D ( 'NONE', #2049, #11504, #6586 ) ;
#8867 = CARTESIAN_POINT ( 'NONE',  ( -16.99999999999998579, -2.249290599286303927, -57.50000000000012079 ) ) ;
#8868 = DIRECTION ( 'NONE',  ( 0.4331347858759544978, 0.9013291614411413910, 0.000000000000000000 ) ) ;
#8869 = CARTESIAN_POINT ( 'NONE',  ( 27.86173033120691400, -68.61243380581731799, -3.657093847832743716 ) ) ;
#8870 = CIRCLE ( 'NONE', #44, 0.7892041907098272802 ) ;
#8871 = AXIS2_PLACEMENT_3D ( 'NONE', #2076, #6766, #7391 ) ;
#8872 = ADVANCED_FACE ( 'NONE', ( #13371 ), #2827, .F. ) ;
#8873 = EDGE_LOOP ( 'NONE', ( #3634, #10402, #9072, #858 ) ) ;
#8874 = CARTESIAN_POINT ( 'NONE',  ( -21.85476584171713199, 5.329050157244537900, 48.00000000000012079 ) ) ;
#8875 = ORIENTED_EDGE ( 'NONE', *, *, #12675, .F. ) ;
#8876 = FACE_OUTER_BOUND ( 'NONE', #14544, .T. ) ;
#8877 = DIRECTION ( 'NONE',  ( 0.000000000000000000, 1.000000000000000000, 0.000000000000000000 ) ) ;
#8878 = ORIENTED_EDGE ( 'NONE', *, *, #7164, .T. ) ;
#8879 = VECTOR ( 'NONE', #14270, 1000.000000000000000 ) ;
#8880 = CARTESIAN_POINT ( 'NONE',  ( -3.190546569013415379, 0.8906624217387615339, -48.00000000000012079 ) ) ;
#8881 = DIRECTION ( 'NONE',  ( 0.000000000000000000, 0.000000000000000000, 1.000000000000000000 ) ) ;
#8882 = EDGE_CURVE ( 'NONE', #6117, #1886, #2963, .T. ) ;
#8883 = AXIS2_PLACEMENT_3D ( 'NONE', #893, #13754, #6595 ) ;
#8884 = EDGE_CURVE ( 'NONE', #2664, #14041, #8853, .T. ) ;
#8885 = VECTOR ( 'NONE', #14925, 1000.000000000000000 ) ;
#8886 = CARTESIAN_POINT ( 'NONE',  ( 12.06814882730127181, -63.62021712493068293, 2.966460067265556777 ) ) ;
#8887 = DIRECTION ( 'NONE',  ( 0.000000000000000000, 0.000000000000000000, -1.000000000000000000 ) ) ;
#8888 = DIRECTION ( 'NONE',  ( -0.8746197071345560570, 0.4848096202550682410, 0.000000000000000000 ) ) ;
#8889 = DIRECTION ( 'NONE',  ( -1.000000000000000000, 0.000000000000000000, 0.000000000000000000 ) ) ;
#8890 = CIRCLE ( 'NONE', #4215, 2.000000000000000000 ) ;
#8891 = VECTOR ( 'NONE', #9826, 1000.000000000000000 ) ;
#8892 = CARTESIAN_POINT ( 'NONE',  ( 68.00000000000001421, -2.249290599286293268, 139.1143251403882459 ) ) ;
#8893 = VECTOR ( 'NONE', #5561, 1000.000000000000000 ) ;
#8894 = ORIENTED_EDGE ( 'NONE', *, *, #10123, .T. ) ;
#8895 = CARTESIAN_POINT ( 'NONE',  ( 88.00000000000002842, 9.769962616701380080E-14, -33.00000000000012790 ) ) ;
#8896 = VERTEX_POINT ( 'NONE', #12762 ) ;
#8897 = VERTEX_POINT ( 'NONE', #3204 ) ;
#8898 = DIRECTION ( 'NONE',  ( 0.5394184268574520047, -0.8420378618367654333, 0.000000000000000000 ) ) ;
#8899 = EDGE_CURVE ( 'NONE', #10987, #11056, #14508, .T. ) ;
#8900 = EDGE_CURVE ( 'NONE', #981, #7221, #3359, .T. ) ;
#8901 = DIRECTION ( 'NONE',  ( 0.000000000000000000, 0.000000000000000000, 1.000000000000000000 ) ) ;
#8902 = PRODUCT_RELATED_PRODUCT_CATEGORY ( 'part', '', ( #5354 ) ) ;
#8903 = CIRCLE ( 'NONE', #7188, 0.7892041907098262810 ) ;
#8904 = CARTESIAN_POINT ( 'NONE',  ( 52.46774229227035136, -1.764205727211077379, 54.56811043785582882 ) ) ;
#8905 = CARTESIAN_POINT ( 'NONE',  ( 84.72310019870096198, 29.52935533987996664, -33.00000000000013500 ) ) ;
#8906 = ORIENTED_EDGE ( 'NONE', *, *, #13485, .F. ) ;
#8907 = VECTOR ( 'NONE', #6689, 1000.000000000000114 ) ;
#8908 = DIRECTION ( 'NONE',  ( -0.000000000000000000, 1.000000000000000000, 1.445602896647339163E-16 ) ) ;
#8909 = ORIENTED_EDGE ( 'NONE', *, *, #15062, .T. ) ;
#8910 = TOROIDAL_SURFACE ( 'NONE', #2282, 3.999999999999996447, 1.000000000000000000 ) ;
#8911 = CARTESIAN_POINT ( 'NONE',  ( -25.21252699837112132, -6.998437922861947769, 57.50000000000012079 ) ) ;
#8912 = CARTESIAN_POINT ( 'NONE',  ( 52.46774229227035136, -1.764205727211077379, 48.51982618741349285 ) ) ;
#8913 = DIRECTION ( 'NONE',  ( -0.000000000000000000, -0.000000000000000000, -1.000000000000000000 ) ) ;
#8914 = SHAPE_REPRESENTATION ( 'Plastic-Headed Retaining Pin', ( #6315 ), #9517 ) ;
#8915 = EDGE_LOOP ( 'NONE', ( #13372, #14350, #14890, #736 ) ) ;
#8916 = CARTESIAN_POINT ( 'NONE',  ( -20.99999999999998579, -2.249290599286302594, -115.4621125123531442 ) ) ;
#8917 = EDGE_LOOP ( 'NONE', ( #7669, #3445, #5330, #5208 ) ) ;
#8918 = VERTEX_POINT ( 'NONE', #5599 ) ;
#8919 = CIRCLE ( 'NONE', #7201, 0.4999999999999995559 ) ;
#8920 = ORIENTED_EDGE ( 'NONE', *, *, #8202, .F. ) ;
#8921 = CIRCLE ( 'NONE', #8681, 4.165819364273509962 ) ;
#8922 = LINE ( 'NONE', #13692, #5476 ) ;
#8923 = CARTESIAN_POINT ( 'NONE',  ( 80.00000000000001421, -74.24929059928631148, 8.000000000000001776 ) ) ;
#8924 = CARTESIAN_POINT ( 'NONE',  ( -24.34296084301338681, 2.966536634491813818, -47.54128347412125066 ) ) ;
#8925 = LINE ( 'NONE', #2544, #8641 ) ;
#8926 = B_SPLINE_CURVE_WITH_KNOTS ( 'NONE', 3,
 ( #15112, #9261, #1250, #4642 ),
 .UNSPECIFIED., .F., .F.,
 ( 4, 4 ),
 ( 0.000000000000000000, 0.006683255761480934656 ),
 .UNSPECIFIED. ) ;
#8927 = EDGE_LOOP ( 'NONE', ( #7586, #1836, #14666, #3203 ) ) ;
#8928 = DIRECTION ( 'NONE',  ( 1.000000000000000000, 0.000000000000000000, 0.000000000000000000 ) ) ;
#8929 = CIRCLE ( 'NONE', #4251, 1.000000000000000888 ) ;
#8930 = CARTESIAN_POINT ( 'NONE',  ( 64.91683959679546945, -11.40731206199988890, 72.41114282892958443 ) ) ;
#8931 = CARTESIAN_POINT ( 'NONE',  ( 33.52235686305655804, -57.48563641131178770, -1.816685854991392457 ) ) ;
#8932 = CARTESIAN_POINT ( 'NONE',  ( -9.101643754575787781, 2.066879234150345024, 47.52815511422343775 ) ) ;
#8933 = CARTESIAN_POINT ( 'NONE',  ( 13.50577566551451092, -66.70046270226328033, -4.174231074487356530 ) ) ;
#8934 = EDGE_CURVE ( 'NONE', #1117, #11541, #15213, .T. ) ;
#8935 = ORIENTED_EDGE ( 'NONE', *, *, #2063, .T. ) ;
#8936 = CARTESIAN_POINT ( 'NONE',  ( 69.46140857195989327, -2.899158388209396975, 73.01624609662880516 ) ) ;
#8937 = EDGE_CURVE ( 'NONE', #9290, #15116, #10368, .T. ) ;
#8938 = EDGE_CURVE ( 'NONE', #7182, #9663, #8725, .T. ) ;
#8939 = DIRECTION ( 'NONE',  ( -0.8420378618367644341, -0.5394184268574535590, -0.000000000000000000 ) ) ;
#8940 = ORIENTED_EDGE ( 'NONE', *, *, #4556, .T. ) ;
#8941 = PRESENTATION_STYLE_ASSIGNMENT (( #14785 ) ) ;
#8942 = CARTESIAN_POINT ( 'NONE',  ( 32.14997420079630785, -58.98766849246936772, -1.832439066039620812 ) ) ;
#8943 = CARTESIAN_POINT ( 'NONE',  ( 64.64681977576807981, -12.79380737173440430, 75.19766410831374515 ) ) ;
#8944 = DIRECTION ( 'NONE',  ( 0.000000000000000000, 1.000000000000000000, 0.000000000000000000 ) ) ;
#8945 = ORIENTED_EDGE ( 'NONE', *, *, #5659, .F. ) ;
#8946 = LINE ( 'NONE', #6343, #8508 ) ;
#8947 = MANIFOLD_SOLID_BREP ( 'Fillet12', #5353 ) ;
#8948 = EDGE_CURVE ( 'NONE', #981, #13646, #12805, .T. ) ;
#8949 = EDGE_CURVE ( 'NONE', #3386, #750, #563, .T. ) ;
#8950 = PLANE ( 'NONE',  #12276 ) ;
#8951 = CARTESIAN_POINT ( 'NONE',  ( 58.00000000000000711, -12.24929059928630970, 38.00000000000012079 ) ) ;
#8952 = DIRECTION ( 'NONE',  ( -0.8746197071345569451, 0.4848096202550666312, 0.000000000000000000 ) ) ;
#8953 = ORIENTED_EDGE ( 'NONE', *, *, #12807, .T. ) ;
#8954 = CARTESIAN_POINT ( 'NONE',  ( 24.27245784421326391, -72.28366650270577054, -6.113054590623763218 ) ) ;
#8955 = VERTEX_POINT ( 'NONE', #10032 ) ;
#8956 = PLANE ( 'NONE',  #3224 ) ;
#8957 = FACE_OUTER_BOUND ( 'NONE', #2716, .T. ) ;
#8958 = VERTEX_POINT ( 'NONE', #10108 ) ;
#8960 = ORIENTED_EDGE ( 'NONE', *, *, #230, .T. ) ;
#8959 = DIRECTION ( 'NONE',  ( -0.000000000000000000, 1.000000000000000000, 1.445602896647339163E-16 ) ) ;
#8961 = PLANE ( 'NONE',  #9526 ) ;
#8962 = CARTESIAN_POINT ( 'NONE',  ( 12.48247979829277199, -64.27177309650438985, 3.135762038898789683 ) ) ;
#8963 = CARTESIAN_POINT ( 'NONE',  ( 10.41145220107785363, -52.71989690418637764, 2.656489712860343744 ) ) ;
#8964 = DIRECTION ( 'NONE',  ( 0.000000000000000000, 0.000000000000000000, -1.000000000000000000 ) ) ;
#8965 = LINE ( 'NONE', #2197, #8138 ) ;
#8966 = CARTESIAN_POINT ( 'NONE',  ( 32.54790116764300478, -57.26105658658105568, 1.816685854991386462 ) ) ;
#8967 = EDGE_CURVE ( 'NONE', #5398, #6058, #12568, .T. ) ;
#8968 = CARTESIAN_POINT ( 'NONE',  ( -24.12409601409935078, -6.885803942510236197, -58.00000000000012079 ) ) ;
#8969 = VERTEX_POINT ( 'NONE', #4320 ) ;
#8970 = FACE_OUTER_BOUND ( 'NONE', #3732, .T. ) ;
#8971 = ORIENTED_EDGE ( 'NONE', *, *, #1237, .F. ) ;
#8972 = CARTESIAN_POINT ( 'NONE',  ( -16.99999999999998579, -2.249290599286303927, -50.50000000000012079 ) ) ;
#8973 = ORIENTED_EDGE ( 'NONE', *, *, #349, .T. ) ;
#8974 = PLANE ( 'NONE',  #5410 ) ;
#8975 = CARTESIAN_POINT ( 'NONE',  ( 69.45693112140031644, -2.708622645674852780, 71.97298415572764441 ) ) ;
#8976 = DIRECTION ( 'NONE',  ( -0.8656763553493069807, -0.5006040828730229375, -0.000000000000000000 ) ) ;
#8977 = DIRECTION ( 'NONE',  ( 0.000000000000000000, -1.000000000000000000, 0.000000000000000000 ) ) ;
#8978 = VERTEX_POINT ( 'NONE', #10186 ) ;
#8979 = CARTESIAN_POINT ( 'NONE',  ( -5.040221427466112125, 4.089237592873837812, -57.50000000000012079 ) ) ;
#8980 = ORIENTED_EDGE ( 'NONE', *, *, #10139, .T. ) ;
#8981 = FACE_OUTER_BOUND ( 'NONE', #3001, .T. ) ;
#8982 = CARTESIAN_POINT ( 'NONE',  ( 8.092697108905420933, -56.34136508318314895, -1.853100783821761466 ) ) ;
#8983 = CARTESIAN_POINT ( 'NONE',  ( 40.00000000000001421, -74.24929059928631148, -33.00000000000000000 ) ) ;
#8984 = ADVANCED_FACE ( 'NONE', ( #12341 ), #2021, .F. ) ;
#8985 = DIRECTION ( 'NONE',  ( 1.000000000000000000, 8.673617379884035472E-17, 0.000000000000000000 ) ) ;
#8986 = EDGE_LOOP ( 'NONE', ( #9543, #79, #5572, #9812 ) ) ;
#8987 = ORIENTED_EDGE ( 'NONE', *, *, #6868, .F. ) ;
#8988 = VECTOR ( 'NONE', #1480, 1000.000000000000000 ) ;
#8989 = CARTESIAN_POINT ( 'NONE',  ( -9.875903985900574611, 2.387222743937553293, -58.00000000000012079 ) ) ;
#8990 = VERTEX_POINT ( 'NONE', #4248 ) ;
#8991 = CARTESIAN_POINT ( 'NONE',  ( 63.43853564383336874, -3.373351419973840581, 54.56811043785582882 ) ) ;
#8992 = VERTEX_POINT ( 'NONE', #628 ) ;
#8993 = ORIENTED_EDGE ( 'NONE', *, *, #14534, .F. ) ;
#8994 = PLANE ( 'NONE',  #1773 ) ;
#8995 = DIRECTION ( 'NONE',  ( 0.000000000000000000, 0.000000000000000000, 1.000000000000000000 ) ) ;
#8996 = CARTESIAN_POINT ( 'NONE',  ( -23.03920594196030791, 4.522656845271360915, -48.26696389624889605 ) ) ;
#8997 = CARTESIAN_POINT ( 'NONE',  ( 33.12442989620986822, -59.21224831720011395, 2.500000000000000000 ) ) ;
#8998 = COLOUR_RGB ( '',0.7921568627450980005, 0.8196078431372548767, 0.9333333333333333481 ) ;
#8999 = DIRECTION ( 'NONE',  ( -0.9971413439177307936, -0.07555885288926501853, 0.000000000000000000 ) ) ;
#9000 = ORIENTED_EDGE ( 'NONE', *, *, #10614, .F. ) ;
#9001 = EDGE_CURVE ( 'NONE', #8619, #3324, #10831, .T. ) ;
#9002 = LINE ( 'NONE', #15011, #3133 ) ;
#9003 = DIRECTION ( 'NONE',  ( 0.4848096202550661871, 0.8746197071345573892, -0.000000000000000000 ) ) ;
#9004 = DIRECTION ( 'NONE',  ( 0.000000000000000000, 0.000000000000000000, -1.000000000000000000 ) ) ;
#9005 = DIRECTION ( 'NONE',  ( -0.000000000000000000, 1.000000000000000000, 1.445602896647339163E-16 ) ) ;
#9006 = CARTESIAN_POINT ( 'NONE',  ( 28.25509448139003155, -61.89662211384294466, 4.174060188878190303 ) ) ;
#9007 = EDGE_LOOP ( 'NONE', ( #389, #2150, #2055, #37 ) ) ;
#9008 = CARTESIAN_POINT ( 'NONE',  ( 69.46363198353849100, -2.410414910243239728, 72.52785177043239173 ) ) ;
#9009 = CIRCLE ( 'NONE', #169, 4.665819364273509073 ) ;
#9010 = VECTOR ( 'NONE', #6060, 1000.000000000000000 ) ;
#9011 = FACE_OUTER_BOUND ( 'NONE', #11817, .T. ) ;
#9012 = ORIENTED_EDGE ( 'NONE', *, *, #4950, .T. ) ;
#9013 = CARTESIAN_POINT ( 'NONE',  ( 21.74884261173415467, -82.24929059928629727, 4.000000000000001776 ) ) ;
#9014 = CARTESIAN_POINT ( 'NONE',  ( 75.52271037289314393, -7.388871293676331220, 71.19766410831374515 ) ) ;
#9015 = EDGE_CURVE ( 'NONE', #13501, #4272, #1717, .T. ) ;
#9016 = DIRECTION ( 'NONE',  ( -0.8746197071345569451, 0.4848096202550666312, 0.000000000000000000 ) ) ;
#9017 = VERTEX_POINT ( 'NONE', #8793 ) ;
#9018 = AXIS2_PLACEMENT_3D ( 'NONE', #5135, #11199, #652 ) ;
#9019 = CARTESIAN_POINT ( 'NONE',  ( 95.31453344691183815, 0.000000000000000000, 33.00000000000012790 ) ) ;
#9020 = PRODUCT_DEFINITION_SHAPE ( 'NONE', 'NONE',  #15232 ) ;
#9021 = VECTOR ( 'NONE', #5584, 1000.000000000000000 ) ;
#9022 = AXIS2_PLACEMENT_3D ( 'NONE', #9781, #14395, #11999 ) ;
#9023 = CIRCLE ( 'NONE', #8763, 9.500000000000001776 ) ;
#9024 = CARTESIAN_POINT ( 'NONE',  ( -8.509932750408504276, 13.28409490805591808, -57.50000000000012079 ) ) ;
#9025 = DIRECTION ( 'NONE',  ( 0.000000000000000000, 0.000000000000000000, 1.000000000000000000 ) ) ;
#9026 = DIRECTION ( 'NONE',  ( -0.8208219420614771833, 0.4549890321264261628, 0.3453061251629969131 ) ) ;
#9027 = CARTESIAN_POINT ( 'NONE',  ( 0.000000000000000000, 21.75070940071322667, 33.00000000000012790 ) ) ;
#9028 = ORIENTED_EDGE ( 'NONE', *, *, #11573, .F. ) ;
#9029 = AXIS2_PLACEMENT_3D ( 'NONE', #3675, #8377, #3051 ) ;
#9030 = ORIENTED_EDGE ( 'NONE', *, *, #10425, .T. ) ;
#9031 = CARTESIAN_POINT ( 'NONE',  ( 32.32247376001314620, -59.70726391082581586, 2.784470044084443430 ) ) ;
#9032 = VERTEX_POINT ( 'NONE', #14870 ) ;
#9033 = ADVANCED_FACE ( 'NONE', ( #862 ), #1860, .F. ) ;
#9034 = DIRECTION ( 'NONE',  ( -0.000000000000000000, -0.000000000000000000, 1.000000000000000000 ) ) ;
#9035 = CARTESIAN_POINT ( 'NONE',  ( 114.6731053250840233, 0.000000000000000000, -13.14990448602693007 ) ) ;
#9036 = CIRCLE ( 'NONE', #13458, 0.5000000000000004441 ) ;
#9037 = EDGE_CURVE ( 'NONE', #10038, #5948, #1495, .T. ) ;
#9038 = AXIS2_PLACEMENT_3D ( 'NONE', #9411, #3480, #4940 ) ;
#9039 = EDGE_CURVE ( 'NONE', #7651, #12307, #14028, .T. ) ;
#9040 = ORIENTED_EDGE ( 'NONE', *, *, #9039, .F. ) ;
#9041 = DIRECTION ( 'NONE',  ( -1.000000000000000000, -1.156482317317870492E-16, 0.000000000000000000 ) ) ;
#9042 = CARTESIAN_POINT ( 'NONE',  ( 23.69232253801246912, -82.24929059928629727, 4.472107801411126182 ) ) ;
#9043 = CARTESIAN_POINT ( 'NONE',  ( 14.04356807543711660, -66.53205946168905882, 4.446982897615813002 ) ) ;
#9044 = EDGE_CURVE ( 'NONE', #7793, #13057, #9329, .T. ) ;
#9045 = CIRCLE ( 'NONE', #11455, 1.000000000000000000 ) ;
#9046 = CARTESIAN_POINT ( 'NONE',  ( 29.69047892279256118, -53.28399145779480506, 4.141535524925028966 ) ) ;
#9047 = CARTESIAN_POINT ( 'NONE',  ( 67.15257324181105503, -7.322644791425992672, 81.40005259842790508 ) ) ;
#9048 = LINE ( 'NONE', #11657, #1254 ) ;
#9049 = AXIS2_PLACEMENT_3D ( 'NONE', #2092, #10421, #7023 ) ;
#9050 = DIRECTION ( 'NONE',  ( 0.000000000000000000, 1.000000000000000000, -0.000000000000000000 ) ) ;
#9051 = DIRECTION ( 'NONE',  ( -0.000000000000000000, -0.000000000000000000, 1.000000000000000000 ) ) ;
#9052 = ORIENTED_EDGE ( 'NONE', *, *, #13197, .F. ) ;
#9053 = DIRECTION ( 'NONE',  ( -0.000000000000000000, 1.000000000000000000, 1.445602896647339163E-16 ) ) ;
#9054 = ORIENTED_EDGE ( 'NONE', *, *, #1656, .T. ) ;
#9055 = CARTESIAN_POINT ( 'NONE',  ( -16.99999999999998579, -2.249290599286303927, -57.50000000000012079 ) ) ;
#9056 = ORIENTED_EDGE ( 'NONE', *, *, #3453, .F. ) ;
#9057 = DIRECTION ( 'NONE',  ( 1.000000000000000000, 0.000000000000000000, 0.000000000000000000 ) ) ;
#9058 = LINE ( 'NONE', #13751, #12697 ) ;
#9059 = DIRECTION ( 'NONE',  ( -0.000000000000000000, -0.000000000000000000, 1.000000000000000000 ) ) ;
#9060 = CARTESIAN_POINT ( 'NONE',  ( 1.004339113574583608, 0.8906624217387615339, -48.50000000000012079 ) ) ;
#9061 = CARTESIAN_POINT ( 'NONE',  ( -30.80945343098651890, -5.389243620311580329, -48.00000000000012079 ) ) ;
#9062 = ORIENTED_EDGE ( 'NONE', *, *, #8, .F. ) ;
#9063 = DIRECTION ( 'NONE',  ( 0.000000000000000000, 0.000000000000000000, -1.000000000000000000 ) ) ;
#9064 = CARTESIAN_POINT ( 'NONE',  ( 8.125939110960342049, -57.15949554451674430, -1.814500213265047623 ) ) ;
#9065 = LINE ( 'NONE', #13759, #8203 ) ;
#9066 = CARTESIAN_POINT ( 'NONE',  ( 33.52235686305655804, -57.48563641131178770, 1.816685854991380911 ) ) ;
#9067 = ORIENTED_EDGE ( 'NONE', *, *, #11099, .T. ) ;
#9068 = ORIENTED_EDGE ( 'NONE', *, *, #4333, .F. ) ;
#9069 = CARTESIAN_POINT ( 'NONE',  ( 62.14930354033766946, 1.441842398587370067, 48.51982618741349285 ) ) ;
#9070 = ORIENTED_EDGE ( 'NONE', *, *, #13520, .T. ) ;
#9071 = DIRECTION ( 'NONE',  ( -0.5394184268574406804, 0.8420378618367728718, 0.000000000000000000 ) ) ;
#9072 = ORIENTED_EDGE ( 'NONE', *, *, #10558, .F. ) ;
#9073 = VERTEX_POINT ( 'NONE', #7647 ) ;
#9074 = ITEM_DEFINED_TRANSFORMATION ( 'NONE', 'NONE', #6800,  #6315 ) ;
#9075 = DIRECTION ( 'NONE',  ( 1.000000000000000000, 0.000000000000000000, 0.000000000000000000 ) ) ;
#9076 = LINE ( 'NONE', #7700, #320 ) ;
#9078 = EDGE_CURVE ( 'NONE', #11277, #8918, #6557, .T. ) ;
#9077 = EDGE_LOOP ( 'NONE', ( #15214, #4750, #8759, #8470 ) ) ;
#9079 = EDGE_CURVE ( 'NONE', #5924, #117, #2194, .T. ) ;
#9080 = CIRCLE ( 'NONE', #12263, 2.000000000000001776 ) ;
#9081 = CIRCLE ( 'NONE', #2450, 2.000000000000000000 ) ;
#9082 = CARTESIAN_POINT ( 'NONE',  ( 117.5294988620952097, -39.82044691928823710, 57.22220354671985376 ) ) ;
#9083 = DIRECTION ( 'NONE',  ( -0.000000000000000000, -1.000000000000000000, 0.000000000000000000 ) ) ;
#9084 = ORIENTED_EDGE ( 'NONE', *, *, #8104, .F. ) ;
#9085 = CARTESIAN_POINT ( 'NONE',  ( 65.00000000000001421, -85.27429059928628874, -22.50000000000000000 ) ) ;
#9086 = CARTESIAN_POINT ( 'NONE',  ( 65.28554636553401735, -11.88096418064013093, 72.74061878094576628 ) ) ;
#9087 = LINE ( 'NONE', #2153, #475 ) ;
#9088 = CARTESIAN_POINT ( 'NONE',  ( 58.00000000000000711, -6.754727345143743733, 36.00000000000012079 ) ) ;
#9089 = CARTESIAN_POINT ( 'NONE',  ( 28.47276934682737703, -58.78589452316695940, 4.200179654085411940 ) ) ;
#9090 = ORIENTED_EDGE ( 'NONE', *, *, #11146, .T. ) ;
#9091 = CARTESIAN_POINT ( 'NONE',  ( 62.35557539207178479, -5.694598376804811402, 54.56811043785582882 ) ) ;
#9092 =( REPRESENTATION_RELATIONSHIP ('NONE','NONE', #15125, #8914 ) REPRESENTATION_RELATIONSHIP_WITH_TRANSFORMATION ( #12542 )SHAPE_REPRESENTATION_RELATIONSHIP( ) );
#9093 = TOROIDAL_SURFACE ( 'NONE', #4924, 1.000000000000000000, 0.5000000000000000000 ) ;
#9094 = LINE ( 'NONE', #771, #7873 ) ;
#9095 = ORIENTED_EDGE ( 'NONE', *, *, #12039, .T. ) ;
#9096 = DIRECTION ( 'NONE',  ( 1.000000000000000000, 0.000000000000000000, 0.000000000000000000 ) ) ;
#9097 =( NAMED_UNIT ( * ) SI_UNIT ( $, .STERADIAN. ) SOLID_ANGLE_UNIT ( ) );
#9098 = ORIENTED_EDGE ( 'NONE', *, *, #4821, .T. ) ;
#9099 = ADVANCED_FACE ( 'NONE', ( #3033, #7725 ), #12410, .F. ) ;
#9100 = EDGE_CURVE ( 'NONE', #996, #1587, #12022, .T. ) ;
#9101 =( NAMED_UNIT ( * ) PLANE_ANGLE_UNIT ( ) SI_UNIT ( $, .RADIAN. ) );
#9102 = DIRECTION ( 'NONE',  ( -1.000000000000000000, -8.673617379884035472E-17, 0.000000000000000000 ) ) ;
#9103 = CARTESIAN_POINT ( 'NONE',  ( 20.86173033120691045, -72.24929059928631148, 0.000000000000000000 ) ) ;
#9104 = EDGE_LOOP ( 'NONE', ( #1080, #13615, #7320, #11727 ) ) ;
#9105 = DIRECTION ( 'NONE',  ( -0.8420378618367728718, -0.5394184268574404584, 0.000000000000000000 ) ) ;
#9106 = VECTOR ( 'NONE', #12401, 1000.000000000000000 ) ;
#9107 = DIRECTION ( 'NONE',  ( -0.8746197071345572782, 0.4848096202550659650, 0.000000000000000000 ) ) ;
#9108 = DIRECTION ( 'NONE',  ( -0.000000000000000000, -0.000000000000000000, 1.000000000000000000 ) ) ;
#9109 = CARTESIAN_POINT ( 'NONE',  ( 8.201103799357262858, -57.48563641131178770, 1.816685854991387794 ) ) ;
#9110 = DIRECTION ( 'NONE',  ( -0.000000000000000000, -0.000000000000000000, -1.000000000000000000 ) ) ;
#9111 = VERTEX_POINT ( 'NONE', #785 ) ;
#9112 = CARTESIAN_POINT ( 'NONE',  ( 33.02271496681120055, -59.65359113318972106, 1.835578343527247691 ) ) ;
#9113 = EDGE_LOOP ( 'NONE', ( #14478, #9248, #5993, #10451 ) ) ;
#9114 = LINE ( 'NONE', #6495, #53 ) ;
#9115 = DIRECTION ( 'NONE',  ( 0.000000000000000000, 0.000000000000000000, 1.000000000000000000 ) ) ;
#9116 = B_SPLINE_CURVE_WITH_KNOTS ( 'NONE', 3,
 ( #11865, #9574, #13174, #12954 ),
 .UNSPECIFIED., .F., .F.,
 ( 4, 4 ),
 ( 0.000000000000000000, 0.006642648484603327214 ),
 .UNSPECIFIED. ) ;
#9117 = EDGE_CURVE ( 'NONE', #4051, #14177, #1214, .T. ) ;
#9118 = ORIENTED_EDGE ( 'NONE', *, *, #15142, .F. ) ;
#9119 = DIRECTION ( 'NONE',  ( 1.000000000000000000, 1.789942591005740441E-15, 0.000000000000000000 ) ) ;
#9120 = CARTESIAN_POINT ( 'NONE',  ( 114.0000000000000284, 19.25070940071369563, -13.14990448602693007 ) ) ;
#9121 = AXIS2_PLACEMENT_3D ( 'NONE', #13515, #7520, #655 ) ;
#9122 = CARTESIAN_POINT ( 'NONE',  ( 109.8334623555409735, 21.75070940071366365, -33.00000000000012790 ) ) ;
#9123 = EDGE_CURVE ( 'NONE', #2463, #10590, #3913, .T. ) ;
#9124 = AXIS2_PLACEMENT_3D ( 'NONE', #1687, #14605, #6452 ) ;
#9125 = B_SPLINE_CURVE_WITH_KNOTS ( 'NONE', 3,
 ( #10866, #1746, #13518, #3128, #2623, #14597, #4045, #2903, #7319, #8975, #14668, #8821, #3780, #11205, #13595, #5527 ),
 .UNSPECIFIED., .F., .F.,
 ( 4, 2, 2, 2, 2, 2, 2, 4 ),
 ( 0.000000000000000000, 0.0003911934542035802576, 0.0007823869084071605152, 0.001173580362610740719, 0.001564773816814321030, 0.002347160725221481004, 0.002738354179425079964, 0.003129547633628678924 ),
 .UNSPECIFIED. ) ;
#9126 = DIRECTION ( 'NONE',  ( -0.000000000000000000, 1.000000000000000000, 1.445602896647339163E-16 ) ) ;
#9127 = CARTESIAN_POINT ( 'NONE',  ( 33.63224119599625794, -56.84162434074946191, -1.823610665447297885 ) ) ;
#9128 = CARTESIAN_POINT ( 'NONE',  ( 0.000000000000000000, -74.24929059928636832, -1.248988969475937798E-13 ) ) ;
#9129 = CARTESIAN_POINT ( 'NONE',  ( -12.33418063572647938, -2.249290599286303927, 50.00000000000012079 ) ) ;
#9130 = CARTESIAN_POINT ( 'NONE',  ( 21.74884261173415467, -82.24929059928629727, 6.000000000000001776 ) ) ;
#9131 = VERTEX_POINT ( 'NONE', #9191 ) ;
#9132 = DIRECTION ( 'NONE',  ( 0.000000000000000000, 0.000000000000000000, -1.000000000000000000 ) ) ;
#9133 = AXIS2_PLACEMENT_3D ( 'NONE', #2663, #6418, #424 ) ;
#9134 = VECTOR ( 'NONE', #8163, 1000.000000000000000 ) ;
#9135 = EDGE_LOOP ( 'NONE', ( #4104, #9480, #4068, #12231 ) ) ;
#9136 = EDGE_CURVE ( 'NONE', #8402, #9446, #9340, .T. ) ;
#9137 = DIRECTION ( 'NONE',  ( 1.000000000000000000, 0.000000000000000000, 0.000000000000000000 ) ) ;
#9138 = AXIS2_PLACEMENT_3D ( 'NONE', #8280, #7969, #15124 ) ;
#9139 = ORIENTED_EDGE ( 'NONE', *, *, #641, .T. ) ;
#9140 = CARTESIAN_POINT ( 'NONE',  ( 30.65234355186507997, 0.000000000000000000, -33.00000000000012790 ) ) ;
#9141 = DIRECTION ( 'NONE',  ( 0.5006040828730246028, -0.8656763553493059815, 0.000000000000000000 ) ) ;
#9142 = CARTESIAN_POINT ( 'NONE',  ( 69.28051765693513175, -4.295678830383773850, 76.19766410831374515 ) ) ;
#9143 = CARTESIAN_POINT ( 'NONE',  ( 4.848008884920353090, 21.49656883983473676, 73.19766410831374515 ) ) ;
#9144 = VERTEX_POINT ( 'NONE', #9109 ) ;
#9145 = CARTESIAN_POINT ( 'NONE',  ( 27.40406279159097380, -67.79239290437253374, -4.531617596075061094 ) ) ;
#9146 = AXIS2_PLACEMENT_3D ( 'NONE', #12715, #3476, #8016 ) ;
#9147 = ORIENTED_EDGE ( 'NONE', *, *, #10466, .T. ) ;
#9148 = VECTOR ( 'NONE', #1379, 1000.000000000000000 ) ;
#9149 = EDGE_CURVE ( 'NONE', #4049, #5382, #4148, .T. ) ;
#9150 = VECTOR ( 'NONE', #11691, 1000.000000000000000 ) ;
#9151 = EDGE_CURVE ( 'NONE', #7221, #56, #5390, .T. ) ;
#9152 = CYLINDRICAL_SURFACE ( 'NONE', #10068, 1.000000000000000888 ) ;
#9153 = CARTESIAN_POINT ( 'NONE',  ( 8.534271205941925231, -54.61739641898338959, -2.842377187921200310 ) ) ;
#9154 = CARTESIAN_POINT ( 'NONE',  ( 63.55116547662790794, -2.088839582009629936, 48.51982618741349285 ) ) ;
#9155 = CARTESIAN_POINT ( 'NONE',  ( 33.12442989620986822, -59.21224831720011395, 1.832439066039631914 ) ) ;
#9156 = ORIENTED_EDGE ( 'NONE', *, *, #12996, .F. ) ;
#9157 = CARTESIAN_POINT ( 'NONE',  ( 108.0866310645538562, 23.25070940071369563, 139.1143251403882459 ) ) ;
#9158 = VERTEX_POINT ( 'NONE', #7958 ) ;
#9159 = DIRECTION ( 'NONE',  ( -0.8656763553492972108, -0.5006040828730397019, 1.548731138869852323E-14 ) ) ;
#9160 = ORIENTED_EDGE ( 'NONE', *, *, #2656, .F. ) ;
#9161 = VECTOR ( 'NONE', #1870, 1000.000000000000000 ) ;
#9162 = AXIS2_PLACEMENT_3D ( 'NONE', #3420, #9115, #12498 ) ;
#9163 = AXIS2_PLACEMENT_3D ( 'NONE', #10714, #7247, #13030 ) ;
#9164 = CARTESIAN_POINT ( 'NONE',  ( 8.691447003131420601, -59.61641240690491372, -2.502824406264639645 ) ) ;
#9165 = DIRECTION ( 'NONE',  ( 0.000000000000000000, 1.000000000000000000, 0.000000000000000000 ) ) ;
#9166 = AXIS2_PLACEMENT_3D ( 'NONE', #12217, #6301, #1748 ) ;
#9167 = CARTESIAN_POINT ( 'NONE',  ( 9.835064211273984114, -54.14139889408635042, -3.328424545751999197 ) ) ;
#9168 = ORIENTED_EDGE ( 'NONE', *, *, #388, .T. ) ;
#9169 = DIRECTION ( 'NONE',  ( 0.000000000000000000, 0.000000000000000000, 1.000000000000000000 ) ) ;
#9170 = LINE ( 'NONE', #1846, #8359 ) ;
#9171 = CYLINDRICAL_SURFACE ( 'NONE', #9188, 0.7892041907098262810 ) ;
#9172 = DIRECTION ( 'NONE',  ( 0.000000000000000000, 0.000000000000000000, 1.000000000000000000 ) ) ;
#9173 = ORIENTED_EDGE ( 'NONE', *, *, #13799, .F. ) ;
#9174 = CIRCLE ( 'NONE', #5494, 4.000000000000000000 ) ;
#9175 = CARTESIAN_POINT ( 'NONE',  ( 69.43268765340762627, -3.261345579701428132, 72.40030056272208014 ) ) ;
#9176 = EDGE_CURVE ( 'NONE', #302, #10002, #11282, .T. ) ;
#9177 = AXIS2_PLACEMENT_3D ( 'NONE', #500, #8520, #8661 ) ;
#9178 = LINE ( 'NONE', #13627, #9106 ) ;
#9179 = ORIENTED_EDGE ( 'NONE', *, *, #5426, .F. ) ;
#9180 = DIRECTION ( 'NONE',  ( 0.000000000000000000, 0.7071067811865965336, 0.7071067811864985009 ) ) ;
#9181 =( LENGTH_UNIT ( ) NAMED_UNIT ( * ) SI_UNIT ( .MILLI., .METRE. ) );
#9182 = CARTESIAN_POINT ( 'NONE',  ( -9.271822474830662131, -6.861803161813125662, -47.50000000000012079 ) ) ;
#9183 = CARTESIAN_POINT ( 'NONE',  ( 64.90552635791956959, 12.46743062497963450, -33.00000000000012790 ) ) ;
#9184 = EDGE_LOOP ( 'NONE', ( #7696, #4178, #13295, #15207 ) ) ;
#9185 = DIRECTION ( 'NONE',  ( 8.673617379884035472E-17, -1.000000000000000000, 0.000000000000000000 ) ) ;
#9186 = VECTOR ( 'NONE', #1733, 1000.000000000000000 ) ;
#9187 = CARTESIAN_POINT ( 'NONE',  ( 33.12582565096496268, -59.20619211347770516, -2.502190571104529138 ) ) ;
#9188 = AXIS2_PLACEMENT_3D ( 'NONE', #13858, #14933, #1154 ) ;
#9189 = DIRECTION ( 'NONE',  ( 0.000000000000000000, 0.000000000000000000, 1.000000000000000000 ) ) ;
#9190 = FACE_OUTER_BOUND ( 'NONE', #15147, .T. ) ;
#9191 = CARTESIAN_POINT ( 'NONE',  ( -80.00000000000001421, -76.24929059928631148, 4.000000000000000000 ) ) ;
#9192 = CARTESIAN_POINT ( 'NONE',  ( 53.04398595309534414, -1.224959495890951100, 60.61639468829817190 ) ) ;
#9193 = EDGE_CURVE ( 'NONE', #6176, #13057, #3257, .T. ) ;
#9194 = ORIENTED_EDGE ( 'NONE', *, *, #6046, .T. ) ;
#9195 = EDGE_CURVE ( 'NONE', #7204, #7606, #12517, .T. ) ;
#9196 = ORIENTED_EDGE ( 'NONE', *, *, #4515, .T. ) ;
#9197 = CARTESIAN_POINT ( 'NONE',  ( 31.67136219134865982, -63.64501252278665788, -2.710939438195376638 ) ) ;
#9198 = VERTEX_POINT ( 'NONE', #14032 ) ;
#9199 = LINE ( 'NONE', #9349, #8879 ) ;
#9200 = CARTESIAN_POINT ( 'NONE',  ( 9.783297955193184237, -53.10754952926042449, 2.473486986449628500 ) ) ;
#9201 = ORIENTED_EDGE ( 'NONE', *, *, #7671, .F. ) ;
#9203 = ORIENTED_EDGE ( 'NONE', *, *, #6796, .T. ) ;
#9202 = CARTESIAN_POINT ( 'NONE',  ( 67.21328690825531282, 25.52935533987996664, 33.00000000000014211 ) ) ;
#9204 = CARTESIAN_POINT ( 'NONE',  ( -12.99999999999998757, -2.249290599286301706, -115.4621125123531442 ) ) ;
#9205 = CARTESIAN_POINT ( 'NONE',  ( 58.00000000000000711, -2.249290599286307479, 33.00000000000012790 ) ) ;
#9206 = DIRECTION ( 'NONE',  ( 0.000000000000000000, 0.000000000000000000, 1.000000000000000000 ) ) ;
#9207 = DIRECTION ( 'NONE',  ( 0.2245701561649794398, -0.9744137433416112382, 0.009279102705852556102 ) ) ;
#9208 = ADVANCED_FACE ( 'NONE', ( #12959 ), #15034, .F. ) ;
#9209 = LINE ( 'NONE', #9513, #6110 ) ;
#9210 = CARTESIAN_POINT ( 'NONE',  ( -22.45192840590307881, 4.946501455397934954, -48.38495513066926890 ) ) ;
#9211 = ORIENTED_EDGE ( 'NONE', *, *, #10079, .T. ) ;
#9212 = CARTESIAN_POINT ( 'NONE',  ( 18.24879706501205590, -53.10810670090265262, -6.494041865157049287 ) ) ;
#9213 = PRODUCT_DEFINITION_CONTEXT ( 'detailed design', #2511, 'design' ) ;
#9214 = ORIENTED_EDGE ( 'NONE', *, *, #11909, .F. ) ;
#9215 = CARTESIAN_POINT ( 'NONE',  ( 18.00000000000001066, 15.25070940071368497, -33.00000000000012790 ) ) ;
#9216 = VERTEX_POINT ( 'NONE', #11643 ) ;
#9217 = CARTESIAN_POINT ( 'NONE',  ( 10.23047706855496308, -60.71197230342421136, -3.050751728647428607 ) ) ;
#9218 = ORIENTED_EDGE ( 'NONE', *, *, #12034, .F. ) ;
#9219 = DIRECTION ( 'NONE',  ( -0.000000000000000000, -0.000000000000000000, -1.000000000000000000 ) ) ;
#9220 = CARTESIAN_POINT ( 'NONE',  ( 16.55198862119230441, -52.24929059928630437, -4.731953141225709203 ) ) ;
#9221 = EDGE_LOOP ( 'NONE', ( #1653, #6871, #1318, #5714 ) ) ;
#9222 = ORIENTED_EDGE ( 'NONE', *, *, #4133, .T. ) ;
#9223 = ADVANCED_FACE ( 'NONE', ( #111 ), #3564, .F. ) ;
#9224 = LINE ( 'NONE', #13908, #9593 ) ;
#9225 = CARTESIAN_POINT ( 'NONE',  ( 11.13720975898229071, -52.41844408481635753, -2.861639392410594507 ) ) ;
#9226 = CARTESIAN_POINT ( 'NONE',  ( 40.00000000000001421, -72.24929059928631148, -32.99999999999999289 ) ) ;
#9227 = CARTESIAN_POINT ( 'NONE',  ( -10.27534025206727186, -8.241935476752797030, 47.97348817130912835 ) ) ;
#9228 = EDGE_LOOP ( 'NONE', ( #7642, #14387, #2917, #12284 ) ) ;
#9229 = VERTEX_POINT ( 'NONE', #5805 ) ;
#9230 = CARTESIAN_POINT ( 'NONE',  ( -3.190546569013415379, 0.8906624217387615339, 48.50000000000012079 ) ) ;
#9231 = VERTEX_POINT ( 'NONE', #5737 ) ;
#9232 = DIRECTION ( 'NONE',  ( -0.9744556954135530358, -0.2245798247307374262, 0.000000000000000000 ) ) ;
#9233 = ORIENTED_EDGE ( 'NONE', *, *, #11996, .F. ) ;
#9234 = VERTEX_POINT ( 'NONE', #10492 ) ;
#9235 = ADVANCED_FACE ( 'NONE', ( #6867 ), #5889, .T. ) ;
#9236 = EDGE_CURVE ( 'NONE', #14170, #13501, #10423, .T. ) ;
#9237 = DIRECTION ( 'NONE',  ( 0.000000000000000000, 0.000000000000000000, 1.000000000000000000 ) ) ;
#9238 = FACE_OUTER_BOUND ( 'NONE', #3826, .T. ) ;
#9239 = DIRECTION ( 'NONE',  ( 0.8420378618367728718, 0.5394184268574404584, 0.000000000000000000 ) ) ;
#9240 = ORIENTED_EDGE ( 'NONE', *, *, #4997, .T. ) ;
#9241 = EDGE_CURVE ( 'NONE', #6995, #6859, #15189, .T. ) ;
#9242 = VECTOR ( 'NONE', #12803, 1000.000000000000000 ) ;
#9243 = DIRECTION ( 'NONE',  ( -0.000000000000000000, -0.000000000000000000, -1.000000000000000000 ) ) ;
#9244 = DIRECTION ( 'NONE',  ( 1.000000000000000000, 0.000000000000000000, 0.000000000000000000 ) ) ;
#9245 = CARTESIAN_POINT ( 'NONE',  ( 32.85051389997479276, -55.70527662866913232, -2.889323894641942392 ) ) ;
#9246 = CARTESIAN_POINT ( 'NONE',  ( -30.80945343098651890, -5.389243620311580329, 48.50000000000012079 ) ) ;
#9247 = CARTESIAN_POINT ( 'NONE',  ( 28.59252212848121033, -57.14744317397804707, 4.208698379002603573 ) ) ;
#9248 = ORIENTED_EDGE ( 'NONE', *, *, #5484, .T. ) ;
#9249 = CARTESIAN_POINT ( 'NONE',  ( 70.25061521000239395, -4.319789889307661390, 72.19766410831373094 ) ) ;
#9250 = ORIENTED_EDGE ( 'NONE', *, *, #2985, .F. ) ;
#9251 = CARTESIAN_POINT ( 'NONE',  ( 96.29968967959054282, 25.52935533987996664, 33.00000000000014211 ) ) ;
#9252 = CIRCLE ( 'NONE', #14897, 10.00000000000000000 ) ;
#9253 = CARTESIAN_POINT ( 'NONE',  ( -9.619661834299611414, -7.413097564672500361, -47.90685900409895481 ) ) ;
#9254 = DIRECTION ( 'NONE',  ( 0.8381289428352243220, 0.5454721580263371949, 0.000000000000000000 ) ) ;
#9255 = ORIENTED_EDGE ( 'NONE', *, *, #5371, .T. ) ;
#9256 = DIRECTION ( 'NONE',  ( -0.5125013958363124900, -0.8586863916854809986, 0.000000000000000000 ) ) ;
#9257 = CARTESIAN_POINT ( 'NONE',  ( 62.67308791069655882, 25.52935533987996664, -33.00000000000013500 ) ) ;
#9258 = EDGE_CURVE ( 'NONE', #7934, #3807, #8926, .T. ) ;
#9259 = LINE ( 'NONE', #15187, #5117 ) ;
#9260 = CARTESIAN_POINT ( 'NONE',  ( -20.99999999999998579, -2.249290599286302594, -115.4621125123531442 ) ) ;
#9261 = CARTESIAN_POINT ( 'NONE',  ( 16.55200847196254088, -52.24929059928630437, -4.731961142181927649 ) ) ;
#9262 = AXIS2_PLACEMENT_3D ( 'NONE', #3076, #14921, #5387 ) ;
#9263 = LINE ( 'NONE', #11401, #286 ) ;
#9264 = CIRCLE ( 'NONE', #9766, 0.5000000000000004441 ) ;
#9265 = ORIENTED_EDGE ( 'NONE', *, *, #2587, .T. ) ;
#9266 = CARTESIAN_POINT ( 'NONE',  ( 121.8927854443908103, -31.94886955507721638, 57.22220354671986087 ) ) ;
#9267 = AXIS2_PLACEMENT_3D ( 'NONE', #9445, #12042, #3516 ) ;
#9268 = ORIENTED_EDGE ( 'NONE', *, *, #9339, .F. ) ;
#9269 = CARTESIAN_POINT ( 'NONE',  ( 8.536817129504960633, -54.60521069725380983, -2.069777907921884985 ) ) ;
#9270 = CARTESIAN_POINT ( 'NONE',  ( 8.673423145672954249, -54.35426670300921614, 2.119310268792462537 ) ) ;
#9271 = AXIS2_PLACEMENT_3D ( 'NONE', #13267, #345, #3797 ) ;
#9272 = VERTEX_POINT ( 'NONE', #13957 ) ;
#9273 = LINE ( 'NONE', #12178, #1640 ) ;
#9274 = DIRECTION ( 'NONE',  ( 0.000000000000000000, 0.000000000000000000, 1.000000000000000000 ) ) ;
#9275 = VECTOR ( 'NONE', #7116, 1000.000000000000000 ) ;
#9276 = EDGE_CURVE ( 'NONE', #8405, #2288, #11134, .T. ) ;
#9277 = EDGE_CURVE ( 'NONE', #2887, #4378, #13266, .T. ) ;
#9278 = CARTESIAN_POINT ( 'NONE',  ( 80.00000000000001421, -74.24929059928631148, 4.000000000000000000 ) ) ;
#9279 = DIRECTION ( 'NONE',  ( 0.3020115420618222357, -0.1674077314120182292, 0.9384901064608630605 ) ) ;
#9280 = VECTOR ( 'NONE', #2044, 1000.000000000000000 ) ;
#9281 = CARTESIAN_POINT ( 'NONE',  ( -28.95977857253349796, -8.587818791446737876, -48.00000000000012079 ) ) ;
#9282 = VECTOR ( 'NONE', #13472, 1000.000000000000000 ) ;
#9283 = DIRECTION ( 'NONE',  ( 0.000000000000000000, -0.000000000000000000, 1.000000000000000000 ) ) ;
#9284 = ADVANCED_FACE ( 'NONE', ( #13400 ), #481, .F. ) ;
#9285 = ORIENTED_EDGE ( 'NONE', *, *, #1130, .T. ) ;
#9286 = CIRCLE ( 'NONE', #2145, 1.000000000000000888 ) ;
#9287 = CARTESIAN_POINT ( 'NONE',  ( 9.126247950560001598, -59.08477032955737940, -2.725562014721529369 ) ) ;
#9288 = EDGE_LOOP ( 'NONE', ( #2050, #8246, #5156, #237 ) ) ;
#9289 = LINE ( 'NONE', #7131, #1986 ) ;
#9290 = VERTEX_POINT ( 'NONE', #1570 ) ;
#9291 = CARTESIAN_POINT ( 'NONE',  ( 13.91363567147297253, -66.07496666188166046, -4.402666029760284871 ) ) ;
#9292 = LINE ( 'NONE', #7698, #4982 ) ;
#9293 = DIRECTION ( 'NONE',  ( -1.000000000000000000, 0.000000000000000000, 0.000000000000000000 ) ) ;
#9294 = VECTOR ( 'NONE', #7141, 1000.000000000000000 ) ;
#9295 = EDGE_CURVE ( 'NONE', #14139, #13981, #13890, .T. ) ;
#9296 = EDGE_CURVE ( 'NONE', #14840, #3763, #13748, .T. ) ;
#9297 = DIRECTION ( 'NONE',  ( 0.000000000000000000, 0.000000000000000000, -1.000000000000000000 ) ) ;
#9298 = AXIS2_PLACEMENT_3D ( 'NONE', #3254, #12645, #8106 ) ;
#9299 = ORIENTED_EDGE ( 'NONE', *, *, #14963, .F. ) ;
#9300 = DIRECTION ( 'NONE',  ( -0.000000000000000000, -0.000000000000000000, -1.000000000000000000 ) ) ;
#9301 = CARTESIAN_POINT ( 'NONE',  ( 10.84100945985316145, -52.50793004641788997, -3.755530264040476407 ) ) ;
#9302 = CARTESIAN_POINT ( 'NONE',  ( 67.21328690825531282, 22.43695620243006772, 33.00000000000014211 ) ) ;
#9303 = DIRECTION ( 'NONE',  ( 0.000000000000000000, 0.000000000000000000, 1.000000000000000000 ) ) ;
#9304 = VERTEX_POINT ( 'NONE', #7560 ) ;
#9305 = DIRECTION ( 'NONE',  ( 1.239088197126290570E-16, -1.000000000000000000, -1.734723475976817547E-15 ) ) ;
#9306 = ORIENTED_EDGE ( 'NONE', *, *, #13741, .F. ) ;
#9307 = DIRECTION ( 'NONE',  ( 0.3020115420618285085, -0.1674077314120178406, 0.9384901064608609511 ) ) ;
#9308 = ORIENTED_EDGE ( 'NONE', *, *, #11666, .F. ) ;
#9309 = ORIENTED_EDGE ( 'NONE', *, *, #1881, .T. ) ;
#9310 = CARTESIAN_POINT ( 'NONE',  ( 60.65595175199513278, -6.557103238384438981, 60.61639468829817190 ) ) ;
#9311 = DIRECTION ( 'NONE',  ( 0.000000000000000000, 0.000000000000000000, -1.000000000000000000 ) ) ;
#9312 = DIRECTION ( 'NONE',  ( -0.5006040828730974335, 0.8656763553492640151, 0.000000000000000000 ) ) ;
#9313 = CARTESIAN_POINT ( 'NONE',  ( -25.46282903980762669, -6.565599745187292946, -48.00000000000012079 ) ) ;
#9314 = ADVANCED_FACE ( 'NONE', ( #621 ), #468, .T. ) ;
#9315 = VERTEX_POINT ( 'NONE', #406 ) ;
#9316 = DIRECTION ( 'NONE',  ( -0.000000000000000000, -0.000000000000000000, -1.000000000000000000 ) ) ;
#9317 = DIRECTION ( 'NONE',  ( 0.000000000000000000, 1.000000000000000000, 0.000000000000000000 ) ) ;
#9318 = ADVANCED_FACE ( 'NONE', ( #3025 ), #5107, .F. ) ;
#9319 = CARTESIAN_POINT ( 'NONE',  ( -16.99999999999998579, -2.249290599286303927, 50.50000000000012079 ) ) ;
#9320 = CARTESIAN_POINT ( 'NONE',  ( 24.36188411769310491, -73.69234276600514022, 6.062089035220985522 ) ) ;
#9321 = VERTEX_POINT ( 'NONE', #1491 ) ;
#9322 = EDGE_CURVE ( 'NONE', #14689, #5446, #14199, .T. ) ;
#9323 = CARTESIAN_POINT ( 'NONE',  ( 14.46725369622999402, -52.24929059928630437, 3.946667064627061627 ) ) ;
#9324 = ORIENTED_EDGE ( 'NONE', *, *, #14052, .F. ) ;
#9325 = CARTESIAN_POINT ( 'NONE',  ( 88.00000000000002842, 9.769962616701380080E-14, 139.1143251403882459 ) ) ;
#9326 = AXIS2_PLACEMENT_3D ( 'NONE', #541, #9947, #12170 ) ;
#9327 = CARTESIAN_POINT ( 'NONE',  ( 119.4687373431154782, -36.32196809074999777, 57.22220354671986797 ) ) ;
#9328 = EDGE_CURVE ( 'NONE', #4038, #10741, #8566, .T. ) ;
#9329 = CIRCLE ( 'NONE', #7854, 0.7892041907098270581 ) ;
#9330 = DIRECTION ( 'NONE',  ( 1.000000000000000000, 0.000000000000000000, 0.000000000000000000 ) ) ;
#9331 = CARTESIAN_POINT ( 'NONE',  ( 58.00000000000000711, -2.249290599286311032, -49.31370849898490150 ) ) ;
#9332 = FACE_OUTER_BOUND ( 'NONE', #3527, .T. ) ;
#9333 = ORIENTED_EDGE ( 'NONE', *, *, #2957, .T. ) ;
#9334 = CARTESIAN_POINT ( 'NONE',  ( -3.190546569013415379, 0.8906624217387615339, -58.00000000000012079 ) ) ;
#9335 = CARTESIAN_POINT ( 'NONE',  ( 31.49298359385885959, -60.71197230342421136, -3.050751728647391747 ) ) ;
#9336 = ADVANCED_FACE ( 'NONE', ( #1710 ), #6402, .F. ) ;
#9337 = DIRECTION ( 'NONE',  ( -0.8420378618367644341, -0.5394184268574535590, -0.000000000000000000 ) ) ;
#9338 = FACE_OUTER_BOUND ( 'NONE', #6076, .T. ) ;
#9339 = EDGE_CURVE ( 'NONE', #8826, #922, #4657, .T. ) ;
#9340 = LINE ( 'NONE', #8027, #13262 ) ;
#9341 = CIRCLE ( 'NONE', #2701, 4.000000000000003553 ) ;
#9342 = AXIS2_PLACEMENT_3D ( 'NONE', #13961, #10268, #3416 ) ;
#9343 = CARTESIAN_POINT ( 'NONE',  ( 37.23881781239525424, 0.000000000000000000, 139.1143251403882459 ) ) ;
#9344 = EDGE_CURVE ( 'NONE', #7395, #11430, #2799, .T. ) ;
#9345 = VERTEX_POINT ( 'NONE', #5258 ) ;
#9346 = DIRECTION ( 'NONE',  ( 0.8208219420614786266, -0.4549890321264268844, -0.3453061251629920281 ) ) ;
#9347 = ADVANCED_FACE ( 'NONE', ( #6336 ), #7869, .F. ) ;
#9348 = VERTEX_POINT ( 'NONE', #7790 ) ;
#9349 = CARTESIAN_POINT ( 'NONE',  ( 96.29968967959054282, 23.25070940071369208, 84.20452624982236500 ) ) ;
#9350 = CARTESIAN_POINT ( 'NONE',  ( 32.52281604437752804, -59.06479067038042530, -2.757123406422443690 ) ) ;
#9351 = VERTEX_POINT ( 'NONE', #5721 ) ;
#9352 = DIRECTION ( 'NONE',  ( -0.8746197071345569451, 0.4848096202550666312, 0.000000000000000000 ) ) ;
#9353 = DIRECTION ( 'NONE',  ( -0.000000000000000000, -0.000000000000000000, -1.000000000000000000 ) ) ;
#9354 = AXIS2_PLACEMENT_3D ( 'NONE', #10137, #14823, #4273 ) ;
#9355 = CARTESIAN_POINT ( 'NONE',  ( 8.091875466796944139, -56.52532528994181860, 2.500000000000000000 ) ) ;
#9356 = DIRECTION ( 'NONE',  ( 0.000000000000000000, 1.000000000000000000, -0.000000000000000000 ) ) ;
#9357 = CARTESIAN_POINT ( 'NONE',  ( -80.00000000000001421, -85.24929059928629727, 8.000000000000001776 ) ) ;
#9358 = CARTESIAN_POINT ( 'NONE',  ( -24.80875755767168300, -6.748058119754043460, 48.36238429206898815 ) ) ;
#9359 = CARTESIAN_POINT ( 'NONE',  ( 10.10275097570081293, -60.61174154192054431, 3.004298789847828388 ) ) ;
#9360 = CARTESIAN_POINT ( 'NONE',  ( 31.29303527934784768, -53.70781053471390720, 3.558938939092266551 ) ) ;
#9361 = ORIENTED_EDGE ( 'NONE', *, *, #14502, .T. ) ;
#9362 = CARTESIAN_POINT ( 'NONE',  ( 12.86711739434182888, -53.69151354811842936, -4.215873134475239148 ) ) ;
#9363 = PRODUCT_DEFINITION_CONTEXT ( 'detailed design', #11431, 'design' ) ;
#9364 = EDGE_CURVE ( 'NONE', #6655, #8652, #5901, .T. ) ;
#9365 = ADVANCED_FACE ( 'NONE', ( #4310 ), #13944, .F. ) ;
#9366 = ORIENTED_EDGE ( 'NONE', *, *, #2292, .T. ) ;
#9367 = DIRECTION ( 'NONE',  ( -0.000000000000000000, -1.000000000000000000, 4.625929269271485914E-16 ) ) ;
#9368 = EDGE_LOOP ( 'NONE', ( #848, #2237, #8749, #7437 ) ) ;
#9369 = ORIENTED_EDGE ( 'NONE', *, *, #13610, .F. ) ;
#9370 = CARTESIAN_POINT ( 'NONE',  ( 65.14946943679815661, -11.22247402132563998, 76.16304653356505128 ) ) ;
#9371 = CYLINDRICAL_SURFACE ( 'NONE', #11439, 10.00000000000000178 ) ;
#9372 = VECTOR ( 'NONE', #3429, 1000.000000000000000 ) ;
#9373 = CARTESIAN_POINT ( 'NONE',  ( -16.99999999999998579, -67.96969602390581144, 33.00000000000001421 ) ) ;
#9374 = EDGE_LOOP ( 'NONE', ( #2435, #150, #1635, #6138 ) ) ;
#9375 = DIRECTION ( 'NONE',  ( 0.8746197071345572782, -0.4848096202550659650, 0.000000000000000000 ) ) ;
#9376 = CARTESIAN_POINT ( 'NONE',  ( 64.11356537587559501, -11.94785244090458498, 82.40005259842790508 ) ) ;
#9377 = CARTESIAN_POINT ( 'NONE',  ( 58.00000000000000711, 0.000000000000000000, 139.1143251403882459 ) ) ;
#9378 = CIRCLE ( 'NONE', #3714, 0.7892041907098270581 ) ;
#9379 = DIRECTION ( 'NONE',  ( 0.4848096202550659650, 0.8746197071345572782, 0.000000000000000000 ) ) ;
#9380 = ORIENTED_EDGE ( 'NONE', *, *, #2415, .F. ) ;
#9381 = ORIENTED_EDGE ( 'NONE', *, *, #2820, .F. ) ;
#9382 = ADVANCED_FACE ( 'NONE', ( #14860 ), #10098, .F. ) ;
#9383 = VECTOR ( 'NONE', #1308, 1000.000000000000000 ) ;
#9384 = AXIS2_PLACEMENT_3D ( 'NONE', #2173, #5731, #13032 ) ;
#9385 = EDGE_CURVE ( 'NONE', #1961, #7020, #5639, .T. ) ;
#9386 = CARTESIAN_POINT ( 'NONE',  ( 32.64893181227846242, -58.48798588983477487, 2.754379989677820717 ) ) ;
#9387 = ORIENTED_EDGE ( 'NONE', *, *, #3670, .T. ) ;
#9388 = LINE ( 'NONE', #13076, #14327 ) ;
#9389 = ORIENTED_EDGE ( 'NONE', *, *, #4519, .T. ) ;
#9390 = ORIENTED_EDGE ( 'NONE', *, *, #901, .F. ) ;
#9391 = VECTOR ( 'NONE', #4803, 1000.000000000000000 ) ;
#9392 = DIRECTION ( 'NONE',  ( 0.000000000000000000, 1.000000000000000000, 0.000000000000000000 ) ) ;
#9393 = DIRECTION ( 'NONE',  ( -0.000000000000000000, 1.000000000000000000, -0.000000000000000000 ) ) ;
#9394 = VECTOR ( 'NONE', #10811, 1000.000000000000000 ) ;
#9395 = PLANE ( 'NONE',  #11335 ) ;
#9396 = CARTESIAN_POINT ( 'NONE',  ( 55.09646579789918519, -6.394265699299607419, 60.61639468829817190 ) ) ;
#9397 = ORIENTED_EDGE ( 'NONE', *, *, #7632, .T. ) ;
#9398 = CARTESIAN_POINT ( 'NONE',  ( 80.00000000000001421, -76.24929059928631148, -6.000000000000000000 ) ) ;
#9399 = DIRECTION ( 'NONE',  ( -0.000000000000000000, 1.000000000000000000, 1.445602896647339163E-16 ) ) ;
#9400 = CARTESIAN_POINT ( 'NONE',  ( 76.16331730212350237, -6.600611445100788899, 72.19766410831374515 ) ) ;
#9401 = PLANE ( 'NONE',  #10574 ) ;
#9402 = ORIENTED_EDGE ( 'NONE', *, *, #13911, .F. ) ;
#9403 = CARTESIAN_POINT ( 'NONE',  ( 62.35557539207178479, -5.694598376804811402, 48.51982618741349285 ) ) ;
#9404 = VECTOR ( 'NONE', #266, 1000.000000000000000 ) ;
#9405 = AXIS2_PLACEMENT_3D ( 'NONE', #313, #9711, #3835 ) ;
#9406 = ORIENTED_EDGE ( 'NONE', *, *, #7287, .T. ) ;
#9407 = VECTOR ( 'NONE', #10847, 1000.000000000000000 ) ;
#9408 = CARTESIAN_POINT ( 'NONE',  ( -16.99999999999998579, -2.249290599286303927, -38.50000000000012790 ) ) ;
#9409 = CARTESIAN_POINT ( 'NONE',  ( -16.99999999999998579, -2.249290599286303927, 48.00000000000012079 ) ) ;
#9410 = DIRECTION ( 'NONE',  ( 0.000000000000000000, 0.000000000000000000, 1.000000000000000000 ) ) ;
#9411 = CARTESIAN_POINT ( 'NONE',  ( 80.00000000000001421, -85.24929059928631148, -6.000000000000001776 ) ) ;
#9412 = CYLINDRICAL_SURFACE ( 'NONE', #3006, 0.7892041907098262810 ) ;
#9413 = ORIENTED_EDGE ( 'NONE', *, *, #11907, .F. ) ;
#9414 = CARTESIAN_POINT ( 'NONE',  ( -80.00000000000001421, -76.24929059928631148, 4.000000000000000000 ) ) ;
#9415 = COLOUR_RGB ( '',0.7921568627450980005, 0.8196078431372548767, 0.9333333333333333481 ) ;
#9416 = LINE ( 'NONE', #10717, #4814 ) ;
#9417 = B_SPLINE_CURVE_WITH_KNOTS ( 'NONE', 3,
 ( #13897, #2114, #5433, #5670, #12753, #2277 ),
 .UNSPECIFIED., .F., .F.,
 ( 4, 2, 4 ),
 ( 0.000000000000000000, 0.0003908577252344191651, 0.0007817154504688383302 ),
 .UNSPECIFIED. ) ;
#9418 = EDGE_CURVE ( 'NONE', #4392, #5446, #10328, .T. ) ;
#9419 = CARTESIAN_POINT ( 'NONE',  ( -16.99999999999998579, -2.249290599286303927, 57.50000000000012079 ) ) ;
#9420 = FACE_OUTER_BOUND ( 'NONE', #1138, .T. ) ;
#9421 = CARTESIAN_POINT ( 'NONE',  ( -24.64146379341137560, -7.004861575982634037, -47.89606589046130125 ) ) ;
#9422 = EDGE_CURVE ( 'NONE', #4285, #844, #13632, .T. ) ;
#9423 = DIRECTION ( 'NONE',  ( 0.8656763553493062036, 0.5006040828730242698, 0.000000000000000000 ) ) ;
#9424 = EDGE_LOOP ( 'NONE', ( #12721, #2475, #11408, #6318 ) ) ;
#9425 =( BOUNDED_SURFACE ( )  B_SPLINE_SURFACE ( 3, 2, ( 
 ( #547, #5253, #690 ),
 ( #7350, #4234, #11309 ),
 ( #7784, #8936, #3086 ),
 ( #1925, #846, #14854 ),
 ( #9008, #1502, #13780 ),
 ( #13712, #5553, #10898 ),
 ( #2394, #9175, #3551 ),
 ( #13861, #2238, #10477 ),
 ( #10323, #15098, #12711 ),
 ( #1235, #8090, #5946 ),
 ( #4548, #5876, #14098 ),
 ( #12946, #7094, #15017 ),
 ( #4785, #10404, #9249 ),
 ( #11459, #924, #3317 ) ),
 .UNSPECIFIED., .F., .F., .F. ) 
 B_SPLINE_SURFACE_WITH_KNOTS ( ( 4, 2, 2, 2, 2, 2, 4 ),
 ( 3, 3 ),
 ( 0.001231944704344905541, 0.001640530120327078883, 0.002049115536309252007, 0.002866286368273598256, 0.003274871784255771381, 0.003683457200237944505, 0.004500628032202290754 ),
 ( 0.000000000000000000, 1.000000000000000000 ),
 .UNSPECIFIED. ) 
 GEOMETRIC_REPRESENTATION_ITEM ( )  RATIONAL_B_SPLINE_SURFACE ( (
 ( 1.000000000000000000, 0.8606282562001420500, 1.000000000000000000),
 ( 1.000000000000000000, 0.8606242962985151124, 1.000000000000000000),
 ( 1.000000000000000000, 0.8593044206441436961, 1.000000000000000000),
 ( 1.000000000000000000, 0.8542070032140108848, 1.000000000000000000),
 ( 1.000000000000000000, 0.8503651661363297309, 1.000000000000000000),
 ( 1.000000000000000000, 0.8359148296423946078, 1.000000000000000000),
 ( 1.000000000000000000, 0.8221039232028367616, 1.000000000000000000),
 ( 1.000000000000000000, 0.7986554744406206829, 1.000000000000000000),
 ( 1.000000000000000000, 0.7902603328760277046, 1.000000000000000000),
 ( 1.000000000000000000, 0.7732499594489120609, 1.000000000000000000),
 ( 1.000000000000000000, 0.7646145331266447354, 1.000000000000000000),
 ( 1.000000000000000000, 0.7387090984038677810, 1.000000000000000000),
 ( 1.000000000000000000, 0.7216377402996817514, 1.000000000000000000),
 ( 1.000000000000000000, 0.7071067811865475727, 1.000000000000000000) ) ) 
 REPRESENTATION_ITEM ( '' )  SURFACE ( )  );
#9426 = EDGE_LOOP ( 'NONE', ( #9617, #8180, #5492, #12376 ) ) ;
#9427 = FACE_OUTER_BOUND ( 'NONE', #12987, .T. ) ;
#9428 = ORIENTED_EDGE ( 'NONE', *, *, #969, .F. ) ;
#9429 = DIRECTION ( 'NONE',  ( 0.000000000000000000, -0.000000000000000000, 1.000000000000000000 ) ) ;
#9430 = CARTESIAN_POINT ( 'NONE',  ( 53.27389963060701916, 0.6670697996139958175, 54.56811043785582882 ) ) ;
#9431 = CIRCLE ( 'NONE', #5745, 0.7892041907098275022 ) ;
#9432 = DIRECTION ( 'NONE',  ( 0.000000000000000000, 1.000000000000000000, -0.000000000000000000 ) ) ;
#9433 = CARTESIAN_POINT ( 'NONE',  ( -3.190546569013415379, 0.8906624217387615339, 57.50000000000012079 ) ) ;
#9434 = CIRCLE ( 'NONE', #2790, 4.665819364273509073 ) ;
#9435 = EDGE_CURVE ( 'NONE', #8992, #5383, #11782, .T. ) ;
#9436 = EDGE_CURVE ( 'NONE', #7093, #10251, #9081, .T. ) ;
#9437 = CARTESIAN_POINT ( 'NONE',  ( 69.45429961572709487, -2.741948779197806996, 76.44472825213317435 ) ) ;
#9438 = CARTESIAN_POINT ( 'NONE',  ( 8.333746545461773181, -58.06117555224668081, -1.821720187977007965 ) ) ;
#9439 = LINE ( 'NONE', #13127, #203 ) ;
#9440 = CARTESIAN_POINT ( 'NONE',  ( 58.00000000000000711, -2.249290599286309256, 77.19766410831374515 ) ) ;
#9441 = CARTESIAN_POINT ( 'NONE',  ( 13.91195367430395713, -69.39711819508848123, 3.980554831151302153 ) ) ;
#9442 = CARTESIAN_POINT ( 'NONE',  ( 32.28464679875084897, -53.39687877504399438, 3.230473295587693361 ) ) ;
#9443 = VECTOR ( 'NONE', #13238, 1000.000000000000000 ) ;
#9444 = VERTEX_POINT ( 'NONE', #3089 ) ;
#9445 = CARTESIAN_POINT ( 'NONE',  ( 58.00000000000000711, -2.249290599286307479, 38.00000000000012079 ) ) ;
#9446 = VERTEX_POINT ( 'NONE', #696 ) ;
#9447 = PLANE ( 'NONE',  #10362 ) ;
#9448 = ORIENTED_EDGE ( 'NONE', *, *, #3944, .T. ) ;
#9449 = ORIENTED_EDGE ( 'NONE', *, *, #3690, .F. ) ;
#9450 = CARTESIAN_POINT ( 'NONE',  ( 65.81665574905483140, -11.71669805552613752, 76.07128683897853705 ) ) ;
#9451 = DIRECTION ( 'NONE',  ( -0.000000000000000000, -0.000000000000000000, -1.000000000000000000 ) ) ;
#9452 = CARTESIAN_POINT ( 'NONE',  ( 23.84527200824996385, -64.01730164816846980, -6.333338579777399779 ) ) ;
#9453 = CARTESIAN_POINT ( 'NONE',  ( 20.86173033120691045, -52.24929059928630437, 0.000000000000000000 ) ) ;
#9454 = EDGE_CURVE ( 'NONE', #6287, #6894, #10250, .T. ) ;
#9455 = DIRECTION ( 'NONE',  ( -1.000000000000000000, 0.000000000000000000, 0.000000000000000000 ) ) ;
#9456 = DIRECTION ( 'NONE',  ( 0.000000000000000000, 1.000000000000000000, 0.000000000000000000 ) ) ;
#9457 = B_SPLINE_CURVE_WITH_KNOTS ( 'NONE', 3,
 ( #7659, #7506, #5050, #14727, #8516, #14443, #2736, #3889 ),
 .UNSPECIFIED., .F., .F.,
 ( 4, 2, 2, 4 ),
 ( 5.262391672463365372E-17, 0.001077686929059507720, 0.002155373858118960796, 0.004310747716237871285 ),
 .UNSPECIFIED. ) ;
#9458 = DIRECTION ( 'NONE',  ( -0.000000000000000000, -0.000000000000000000, -1.000000000000000000 ) ) ;
#9459 = ORIENTED_EDGE ( 'NONE', *, *, #12327, .T. ) ;
#9460 = ORIENTED_EDGE ( 'NONE', *, *, #12243, .T. ) ;
#9461 = CARTESIAN_POINT ( 'NONE',  ( -24.96222495693456978, -7.431276100536581275, -57.50000000000012079 ) ) ;
#9462 = VERTEX_POINT ( 'NONE', #774 ) ;
#9463 = CARTESIAN_POINT ( 'NONE',  ( 9.236751385704064177, -59.22992907132844920, -2.757908842764468016 ) ) ;
#9464 = ORIENTED_EDGE ( 'NONE', *, *, #13244, .F. ) ;
#9465 = FACE_OUTER_BOUND ( 'NONE', #10841, .T. ) ;
#9466 = MANIFOLD_SOLID_BREP ( 'Cut-Extrude3', #12982 ) ;
#9467 = ORIENTED_EDGE ( 'NONE', *, *, #11176, .F. ) ;
#9468 = LINE ( 'NONE', #2461, #8750 ) ;
#9469 = CARTESIAN_POINT ( 'NONE',  ( 130.4454129427046496, -1.749290599286305259, -13.14990448602692474 ) ) ;
#9470 = VERTEX_POINT ( 'NONE', #9251 ) ;
#9471 = CARTESIAN_POINT ( 'NONE',  ( 64.90552635791956959, 12.46743062497963450, 33.00000000000014211 ) ) ;
#9472 = DIRECTION ( 'NONE',  ( 1.110223024625156540E-15, -1.000000000000000000, 0.000000000000000000 ) ) ;
#9473 = ORIENTED_EDGE ( 'NONE', *, *, #13825, .T. ) ;
#9474 = ADVANCED_FACE ( 'NONE', ( #4239 ), #11467, .T. ) ;
#9475 = CARTESIAN_POINT ( 'NONE',  ( -16.99999999999998579, -2.249290599286303927, 50.50000000000012079 ) ) ;
#9476 = CARTESIAN_POINT ( 'NONE',  ( -9.456839514482961562, 2.659958822950721391, -48.37147253714708484 ) ) ;
#9477 = DIRECTION ( 'NONE',  ( 0.000000000000000000, 0.000000000000000000, -1.000000000000000000 ) ) ;
#9478 = ORIENTED_EDGE ( 'NONE', *, *, #9548, .T. ) ;
#9479 = CARTESIAN_POINT ( 'NONE',  ( 108.0866310645538562, 21.75070940071366365, 139.1143251403882459 ) ) ;
#9480 = ORIENTED_EDGE ( 'NONE', *, *, #9258, .F. ) ;
#9481 = PLANE ( 'NONE',  #2265 ) ;
#9482 = DIRECTION ( 'NONE',  ( -0.3738365665314423159, 0.000000000000000000, 0.9274945937977119303 ) ) ;
#9483 = ORIENTED_EDGE ( 'NONE', *, *, #11943, .F. ) ;
#9484 =( LENGTH_UNIT ( ) NAMED_UNIT ( * ) SI_UNIT ( .MILLI., .METRE. ) );
#9485 = CARTESIAN_POINT ( 'NONE',  ( 9.200644618036294631, -59.06479067038042530, 2.757123406423259038 ) ) ;
#9486 = CARTESIAN_POINT ( 'NONE',  ( 29.66000553811798568, -63.57773214734889677, 2.964070158660705445 ) ) ;
#9487 = ORIENTED_EDGE ( 'NONE', *, *, #2930, .F. ) ;
#9488 = EDGE_CURVE ( 'NONE', #12270, #10980, #4324, .T. ) ;
#9489 = CARTESIAN_POINT ( 'NONE',  ( -3.190546569013415379, 0.8906624217387615339, -48.50000000000012079 ) ) ;
#9490 = CIRCLE ( 'NONE', #3334, 2.500000000000002220 ) ;
#9491 = MANIFOLD_SOLID_BREP ( 'Boss-Extrude18', #2154 ) ;
#9492 = AXIS2_PLACEMENT_3D ( 'NONE', #6864, #1012, #5802 ) ;
#9493 = CARTESIAN_POINT ( 'NONE',  ( 31.96861646306723514, -60.26934622950980724, -2.884867303495886048 ) ) ;
#9494 = CARTESIAN_POINT ( 'NONE',  ( 80.00000000000001421, -74.24929059928631148, -4.000000000000000000 ) ) ;
#9495 = CARTESIAN_POINT ( 'NONE',  ( 29.25256031600680018, -63.08803683229670156, 3.873126822354365562 ) ) ;
#9496 = CARTESIAN_POINT ( 'NONE',  ( 117.2274873200333900, -39.65303918787621740, 56.28371344025897116 ) ) ;
#9497 = CARTESIAN_POINT ( 'NONE',  ( 31.59592920804998073, -53.91129217357566716, -3.442845340291982303 ) ) ;
#9498 = ORIENTED_EDGE ( 'NONE', *, *, #8304, .F. ) ;
#9499 = AXIS2_PLACEMENT_3D ( 'NONE', #9327, #15174, #11704 ) ;
#9500 = CARTESIAN_POINT ( 'NONE',  ( -30.80945343098651890, -5.389243620311580329, -48.00000000000012079 ) ) ;
#9501 = EDGE_CURVE ( 'NONE', #3720, #13863, #6535, .T. ) ;
#9502 = ORIENTED_EDGE ( 'NONE', *, *, #13363, .T. ) ;
#9503 = CARTESIAN_POINT ( 'NONE',  ( 12.08912955200521822, -52.24929059928630437, -3.123959181890475278 ) ) ;
#9504 = CARTESIAN_POINT ( 'NONE',  ( 58.80593636315131079, 3.245402227105440129, 60.61639468829817190 ) ) ;
#9505 = CARTESIAN_POINT ( 'NONE',  ( 18.03113812440135888, -85.24929059928631148, 4.472107801411127959 ) ) ;
#9506 = CARTESIAN_POINT ( 'NONE',  ( -16.99999999999998579, -2.249290599286303927, -47.50000000000012079 ) ) ;
#9507 = CARTESIAN_POINT ( 'NONE',  ( 69.42475957733114456, -3.331272038940554570, 76.03737743669417171 ) ) ;
#9508 = VECTOR ( 'NONE', #3461, 1000.000000000000000 ) ;
#9509 = AXIS2_PLACEMENT_3D ( 'NONE', #10369, #12673, #9141 ) ;
#9510 = EDGE_CURVE ( 'NONE', #13766, #12779, #10724, .T. ) ;
#9511 = LINE ( 'NONE', #47, #12997 ) ;
#9512 = CARTESIAN_POINT ( 'NONE',  ( -24.54316049702162772, -7.158540003846257882, 48.36906329404664007 ) ) ;
#9513 = CARTESIAN_POINT ( 'NONE',  ( 80.00000000000001421, -74.24929059928631148, -32.00000000000000000 ) ) ;
#9514 = CIRCLE ( 'NONE', #6573, 1.000000000000000888 ) ;
#9515 = CARTESIAN_POINT ( 'NONE',  ( 32.44794091343229780, -53.56780286158647186, 2.317958153238739882 ) ) ;
#9516 = EDGE_CURVE ( 'NONE', #6563, #9615, #6061, .T. ) ;
#9517 =( GEOMETRIC_REPRESENTATION_CONTEXT ( 3 ) GLOBAL_UNCERTAINTY_ASSIGNED_CONTEXT ( ( #15209 ) ) GLOBAL_UNIT_ASSIGNED_CONTEXT ( ( #9484, #103, #15176 ) ) REPRESENTATION_CONTEXT ( 'NONE', 'WORKASPACE' ) );
#9518 = EDGE_LOOP ( 'NONE', ( #3297, #9459, #14161, #10523 ) ) ;
#9519 = EDGE_CURVE ( 'NONE', #1506, #1905, #8408, .T. ) ;
#9520 = EDGE_CURVE ( 'NONE', #14454, #6912, #2374, .T. ) ;
#9521 = LINE ( 'NONE', #10818, #10256 ) ;
#9522 = EDGE_LOOP ( 'NONE', ( #3900, #12354, #12636, #2240 ) ) ;
#9523 = CARTESIAN_POINT ( 'NONE',  ( 8.466388912403532530, -58.63671304798791084, 1.826958385055444722 ) ) ;
#9524 = AXIS2_PLACEMENT_3D ( 'NONE', #4960, #6047, #10731 ) ;
#9525 = ORIENTED_EDGE ( 'NONE', *, *, #2396, .T. ) ;
#9526 = AXIS2_PLACEMENT_3D ( 'NONE', #14805, #6424, #8804 ) ;
#9527 = ORIENTED_EDGE ( 'NONE', *, *, #6285, .F. ) ;
#9528 = CARTESIAN_POINT ( 'NONE',  ( 65.88651289459839688, -11.69095208493818738, 76.10064029115018513 ) ) ;
#9529 = CARTESIAN_POINT ( 'NONE',  ( 96.29968967959054282, 23.25070940071369208, -33.00000000000012790 ) ) ;
#9530 = EDGE_CURVE ( 'NONE', #10346, #7613, #5950, .T. ) ;
#9531 = DIRECTION ( 'NONE',  ( 0.000000000000000000, -0.000000000000000000, 1.000000000000000000 ) ) ;
#9532 = VERTEX_POINT ( 'NONE', #12798 ) ;
#9533 = APPLICATION_CONTEXT ( 'automotive_design' ) ;
#9534 = VECTOR ( 'NONE', #7294, 1000.000000000000000 ) ;
#9535 = CARTESIAN_POINT ( 'NONE',  ( 8.688475229799015764, -54.32282595323670904, 2.125007313488405991 ) ) ;
#9536 = AXIS2_PLACEMENT_3D ( 'NONE', #7778, #13704, #1919 ) ;
#9537 = CARTESIAN_POINT ( 'NONE',  ( 50.01091543003727224, 23.25070940071368852, 33.00000000000012790 ) ) ;
#9538 = DIRECTION ( 'NONE',  ( 0.000000000000000000, 0.000000000000000000, -1.000000000000000000 ) ) ;
#9539 = VERTEX_POINT ( 'NONE', #10562 ) ;
#9540 = EDGE_LOOP ( 'NONE', ( #4637, #4046, #14578, #9361, #3740, #9309, #11836, #11645, #13152, #3055 ) ) ;
#9541 = ADVANCED_FACE ( 'NONE', ( #4708 ), #5570, .T. ) ;
#9542 = DIRECTION ( 'NONE',  ( 0.000000000000000000, -1.000000000000000000, -2.312964634635740689E-15 ) ) ;
#9543 = ORIENTED_EDGE ( 'NONE', *, *, #6195, .F. ) ;
#9544 = DIRECTION ( 'NONE',  ( -0.000000000000000000, -0.000000000000000000, -1.000000000000000000 ) ) ;
#9545 = AXIS2_PLACEMENT_3D ( 'NONE', #3820, #13001, #9538 ) ;
#9546 = ORIENTED_EDGE ( 'NONE', *, *, #4821, .F. ) ;
#9547 = CARTESIAN_POINT ( 'NONE',  ( 30.84433510184845773, -61.22098757969700955, 3.286659897587124401 ) ) ;
#9548 = EDGE_CURVE ( 'NONE', #13009, #9321, #8519, .T. ) ;
#9549 = ORIENTED_EDGE ( 'NONE', *, *, #10598, .T. ) ;
#9550 = CIRCLE ( 'NONE', #6823, 0.7892041907098261699 ) ;
#9551 = VECTOR ( 'NONE', #2168, 1000.000000000000000 ) ;
#9552 = LINE ( 'NONE', #14084, #6788 ) ;
#9553 = CARTESIAN_POINT ( 'NONE',  ( 60.34603303165619792, -7.282908750500069139, 54.56811043785583593 ) ) ;
#9554 = ORIENTED_EDGE ( 'NONE', *, *, #4794, .T. ) ;
#9555 = CARTESIAN_POINT ( 'NONE',  ( 4.848008884920353090, 21.49656883983473676, 75.19766410831374515 ) ) ;
#9556 = CARTESIAN_POINT ( 'NONE',  ( 70.26445833701072274, -4.474174595298148205, 72.19766410831374515 ) ) ;
#9557 = EDGE_LOOP ( 'NONE', ( #209, #6915, #12633, #6526 ) ) ;
#9558 = VECTOR ( 'NONE', #12383, 1000.000000000000000 ) ;
#9559 = DIRECTION ( 'NONE',  ( 0.000000000000000000, -4.625929269271485914E-16, -1.000000000000000000 ) ) ;
#9560 = CARTESIAN_POINT ( 'NONE',  ( -9.041069614211208361, 1.954516911250973932, -47.50000000000011369 ) ) ;
#9561 = DIRECTION ( 'NONE',  ( 1.000000000000000000, 0.000000000000000000, 0.000000000000000000 ) ) ;
#9562 = CIRCLE ( 'NONE', #5367, 4.000000000000000000 ) ;
#9563 = ORIENTED_EDGE ( 'NONE', *, *, #3488, .T. ) ;
#9564 = CARTESIAN_POINT ( 'NONE',  ( -22.95637227168126770, 4.533106128208347130, 48.03392779025640635 ) ) ;
#9565 = EDGE_CURVE ( 'NONE', #6058, #8849, #5819, .T. ) ;
#9566 = ORIENTED_EDGE ( 'NONE', *, *, #706, .T. ) ;
#9567 = EDGE_CURVE ( 'NONE', #505, #12008, #4067, .T. ) ;
#9568 = DIRECTION ( 'NONE',  ( 1.000000000000000000, 0.000000000000000000, 0.000000000000000000 ) ) ;
#9569 = CARTESIAN_POINT ( 'NONE',  ( -21.85476584171713199, 5.329050157244537900, -48.00000000000012079 ) ) ;
#9570 = EDGE_LOOP ( 'NONE', ( #9381, #6735, #10861, #2201 ) ) ;
#9571 = VERTEX_POINT ( 'NONE', #249 ) ;
#9572 = DIRECTION ( 'NONE',  ( 0.000000000000000000, 0.000000000000000000, 1.000000000000000000 ) ) ;
#9573 = CARTESIAN_POINT ( 'NONE',  ( -12.14523415828302078, -9.827631355817260328, -48.50000000000012079 ) ) ;
#9574 = CARTESIAN_POINT ( 'NONE',  ( 25.53228516887957511, -53.25924485586082113, -5.664696970550253674 ) ) ;
#9575 = CARTESIAN_POINT ( 'NONE',  ( -9.107478285483566083, 2.086796655788927701, -48.09696226170978406 ) ) ;
#9576 = CARTESIAN_POINT ( 'NONE',  ( 6.810513572378962266, -47.87885576612686123, 2.732387392847887231 ) ) ;
#9577 = AXIS2_PLACEMENT_3D ( 'NONE', #12081, #6090, #8611 ) ;
#9578 = DIRECTION ( 'NONE',  ( 0.000000000000000000, -0.000000000000000000, 1.000000000000000000 ) ) ;
#9579 = CARTESIAN_POINT ( 'NONE',  ( 62.67308791069655882, 29.52935533987996664, 33.00000000000014211 ) ) ;
#9580 = CARTESIAN_POINT ( 'NONE',  ( 33.52235686305655804, -57.48563641131178770, 1.816685854991380911 ) ) ;
#9581 = CARTESIAN_POINT ( 'NONE',  ( 31.78656436043918987, -54.06072418659015000, -3.368302239731141512 ) ) ;
#9582 = EDGE_CURVE ( 'NONE', #7515, #1460, #9645, .T. ) ;
#9583 = ADVANCED_FACE ( 'NONE', ( #14102 ), #3554, .T. ) ;
#9584 = VERTEX_POINT ( 'NONE', #14745 ) ;
#9585 = PRODUCT_RELATED_PRODUCT_CATEGORY ( 'part', '', ( #14949 ) ) ;
#9586 = DIRECTION ( 'NONE',  ( 1.000000000000000000, 1.156482317317870492E-16, 0.000000000000000000 ) ) ;
#9587 = LINE ( 'NONE', #15195, #9404 ) ;
#9588 = ORIENTED_EDGE ( 'NONE', *, *, #14373, .T. ) ;
#9589 = CARTESIAN_POINT ( 'NONE',  ( 40.33162949095117966, 0.000000000000000000, -33.00000000000012790 ) ) ;
#9590 = CARTESIAN_POINT ( 'NONE',  ( 119.1667258010536301, -36.15456035933797807, 56.28371344025897827 ) ) ;
#9591 = DIRECTION ( 'NONE',  ( 1.000000000000000000, 0.000000000000000000, 0.000000000000000000 ) ) ;
#9592 = DIRECTION ( 'NONE',  ( -1.000000000000000000, 0.000000000000000000, 0.000000000000000000 ) ) ;
#9593 = VECTOR ( 'NONE', #7917, 1000.000000000000000 ) ;
#9594 = VECTOR ( 'NONE', #9955, 1000.000000000000000 ) ;
#9595 = DIRECTION ( 'NONE',  ( 9.912705577010325549E-17, -1.000000000000000000, 0.000000000000000000 ) ) ;
#9596 = CARTESIAN_POINT ( 'NONE',  ( -25.21252699939434194, -6.998437923453657561, 48.43453164808065736 ) ) ;
#9597 = DIRECTION ( 'NONE',  ( 0.9274945937977119303, 1.645879719650006166E-15, -0.3738365665314420383 ) ) ;
#9598 = VERTEX_POINT ( 'NONE', #1472 ) ;
#9599 = CARTESIAN_POINT ( 'NONE',  ( -1.197457146693684082, -2.220571218158921223, -58.00000000000012079 ) ) ;
#9600 = ORIENTED_EDGE ( 'NONE', *, *, #10206, .T. ) ;
#9601 = CARTESIAN_POINT ( 'NONE',  ( 14.11897691353965811, -53.27035328036003392, 4.884026039770247074 ) ) ;
#9602 = AXIS2_PLACEMENT_3D ( 'NONE', #12344, #11254, #13348 ) ;
#9603 = ORIENTED_EDGE ( 'NONE', *, *, #4449, .T. ) ;
#9605 = ORIENTED_EDGE ( 'NONE', *, *, #9385, .F. ) ;
#9604 = CARTESIAN_POINT ( 'NONE',  ( 64.11356538205144773, -11.94785243701160127, 75.33582547088241199 ) ) ;
#9606 = EDGE_CURVE ( 'NONE', #12466, #9700, #12370, .T. ) ;
#9607 = FACE_OUTER_BOUND ( 'NONE', #12392, .T. ) ;
#9608 = CARTESIAN_POINT ( 'NONE',  ( 80.00000000000001421, -76.24929059928631148, 4.000000000000000000 ) ) ;
#9609 = ORIENTED_EDGE ( 'NONE', *, *, #5463, .F. ) ;
#9610 = CARTESIAN_POINT ( 'NONE',  ( 8.089025167907525571, -56.24768769701488935, 2.562823873652622542 ) ) ;
#9611 = AXIS2_PLACEMENT_3D ( 'NONE', #8740, #3127, #6588 ) ;
#9612 = CARTESIAN_POINT ( 'NONE',  ( -25.15752072101212278, 2.619472661158555038, 48.00000000000012079 ) ) ;
#9613 = CYLINDRICAL_SURFACE ( 'NONE', #12980, 4.000000000000000000 ) ;
#9614 = EDGE_CURVE ( 'NONE', #3355, #3566, #8486, .T. ) ;
#9615 = VERTEX_POINT ( 'NONE', #7751 ) ;
#9616 = EDGE_CURVE ( 'NONE', #12776, #7020, #5076, .T. ) ;
#9617 = ORIENTED_EDGE ( 'NONE', *, *, #14583, .F. ) ;
#9618 = LINE ( 'NONE', #14301, #4085 ) ;
#9619 = VERTEX_POINT ( 'NONE', #12007 ) ;
#9620 = CARTESIAN_POINT ( 'NONE',  ( -12.99999999999998757, -2.249290599286303927, 38.00000000000012079 ) ) ;
#9621 = EDGE_LOOP ( 'NONE', ( #3157, #11702, #13429, #10208 ) ) ;
#9622 = FACE_OUTER_BOUND ( 'NONE', #9833, .T. ) ;
#9623 = CIRCLE ( 'NONE', #8094, 8.500000000000000000 ) ;
#9624 = EDGE_LOOP ( 'NONE', ( #7845, #12078, #7755, #8336 ) ) ;
#9625 = CARTESIAN_POINT ( 'NONE',  ( 67.21328690825529861, 29.52935533987996664, -21.00807340887166674 ) ) ;
#9626 = CARTESIAN_POINT ( 'NONE',  ( -10.08762850755046969, -8.023634329963208245, 47.66527511103321046 ) ) ;
#9627 = ORIENTED_EDGE ( 'NONE', *, *, #13050, .F. ) ;
#9628 = EDGE_CURVE ( 'NONE', #5320, #8533, #14640, .T. ) ;
#9629 = ADVANCED_FACE ( 'NONE', ( #6179 ), #5366, .T. ) ;
#9630 = CARTESIAN_POINT ( 'NONE',  ( 73.69809405469877106, 29.52935533987996664, -27.49288055531513209 ) ) ;
#9631 = CARTESIAN_POINT ( 'NONE',  ( 69.99947051259638897, -3.232128232595322448, 72.90093656932181432 ) ) ;
#9632 = CIRCLE ( 'NONE', #5688, 4.505436745857433145 ) ;
#9633 = ORIENTED_EDGE ( 'NONE', *, *, #14778, .F. ) ;
#9634 = VECTOR ( 'NONE', #14720, 1000.000000000000000 ) ;
#9635 = VECTOR ( 'NONE', #5710, 1000.000000000000000 ) ;
#9636 = CARTESIAN_POINT ( 'NONE',  ( 80.00000000000001421, -85.24929059928629727, 32.00000000000000000 ) ) ;
#9637 = LINE ( 'NONE', #5941, #5441 ) ;
#9638 = DIRECTION ( 'NONE',  ( 0.8908241094534407045, 0.4543483311474627029, 0.000000000000000000 ) ) ;
#9639 = ORIENTED_EDGE ( 'NONE', *, *, #13649, .T. ) ;
#9640 = DIRECTION ( 'NONE',  ( -1.224646799147353207E-16, 1.000000000000000000, 0.000000000000000000 ) ) ;
#9641 = VECTOR ( 'NONE', #14506, 1000.000000000000000 ) ;
#9642 = ORIENTED_EDGE ( 'NONE', *, *, #9151, .T. ) ;
#9643 = VECTOR ( 'NONE', #4383, 1000.000000000000000 ) ;
#9644 = PLANE ( 'NONE',  #9653 ) ;
#9645 = LINE ( 'NONE', #3398, #5313 ) ;
#9646 = ORIENTED_EDGE ( 'NONE', *, *, #10279, .T. ) ;
#9647 = VECTOR ( 'NONE', #14126, 1000.000000000000000 ) ;
#9648 = PRODUCT_CONTEXT ( 'NONE', #11879, 'mechanical' ) ;
#9649 = CARTESIAN_POINT ( 'NONE',  ( 8.464703746084037306, -58.62940108252750093, 2.501915095506599407 ) ) ;
#9650 = CARTESIAN_POINT ( 'NONE',  ( 27.86173033120691400, -68.61243380581734641, 3.657093847832750377 ) ) ;
#9651 = CARTESIAN_POINT ( 'NONE',  ( -9.148597373295839219, 2.167486929505451076, -48.18452149279841024 ) ) ;
#9652 = FACE_OUTER_BOUND ( 'NONE', #13673, .T. ) ;
#9653 = AXIS2_PLACEMENT_3D ( 'NONE', #2781, #167, #13318 ) ;
#9654 = CARTESIAN_POINT ( 'NONE',  ( 100.1541764164548880, 23.25070940071369208, -33.00000000000012790 ) ) ;
#9655 = LINE ( 'NONE', #9579, #10802 ) ;
#9656 = VECTOR ( 'NONE', #10658, 1000.000000000000000 ) ;
#9657 = ADVANCED_FACE ( 'NONE', ( #13437 ), #14826, .F. ) ;
#9658 = DIRECTION ( 'NONE',  ( 0.000000000000000000, 1.000000000000000000, 0.000000000000000000 ) ) ;
#9659 = DIRECTION ( 'NONE',  ( 0.000000000000000000, -1.000000000000000000, 0.000000000000000000 ) ) ;
#9660 = AXIS2_PLACEMENT_3D ( 'NONE', #1418, #14359, #4962 ) ;
#9661 = EDGE_CURVE ( 'NONE', #11505, #1679, #4274, .T. ) ;
#9662 = DIRECTION ( 'NONE',  ( -0.000000000000000000, 0.000000000000000000, -1.000000000000000000 ) ) ;
#9663 = VERTEX_POINT ( 'NONE', #7677 ) ;
#9664 = CARTESIAN_POINT ( 'NONE',  ( 84.72310019870096198, 25.52935533987996664, 33.00000000000014211 ) ) ;
#9665 = CARTESIAN_POINT ( 'NONE',  ( 31.49298359385885959, -60.71197230342421136, -3.050751728647420613 ) ) ;
#9666 = AXIS2_PLACEMENT_3D ( 'NONE', #13353, #428, #8802 ) ;
#9667 = CARTESIAN_POINT ( 'NONE',  ( 118.2606911748681568, -35.65233716510192608, 53.46824312087640863 ) ) ;
#9668 = DIRECTION ( 'NONE',  ( -0.000000000000000000, -0.000000000000000000, -1.000000000000000000 ) ) ;
#9669 = AXIS2_PLACEMENT_3D ( 'NONE', #12801, #856, #10254 ) ;
#9670 = CARTESIAN_POINT ( 'NONE',  ( 88.00000000000000000, 23.25070940071369208, 84.20452624982236500 ) ) ;
#9671 = CARTESIAN_POINT ( 'NONE',  ( 64.34486446596575604, -11.79842398862770736, 72.19615287623349786 ) ) ;
#9672 = AXIS2_PLACEMENT_3D ( 'NONE', #5200, #11901, #14584 ) ;
#9673 = EDGE_CURVE ( 'NONE', #246, #531, #7832, .T. ) ;
#9674 = CARTESIAN_POINT ( 'NONE',  ( 70.22985855910454234, -4.172664678593861254, 76.17430469024502315 ) ) ;
#9675 = CARTESIAN_POINT ( 'NONE',  ( -65.00000000000001421, -87.24929059928631148, 19.99999999999999645 ) ) ;
#9676 = EDGE_CURVE ( 'NONE', #1446, #4646, #813, .T. ) ;
#9677 = CARTESIAN_POINT ( 'NONE',  ( 29.35555050496136076, -52.24929059928631148, 3.199931146564416462 ) ) ;
#9678 = ORIENTED_EDGE ( 'NONE', *, *, #4228, .T. ) ;
#9679 = AXIS2_PLACEMENT_3D ( 'NONE', #12301, #1756, #1128 ) ;
#9680 = DIRECTION ( 'NONE',  ( 0.000000000000000000, 0.000000000000000000, 1.000000000000000000 ) ) ;
#9681 = UNCERTAINTY_MEASURE_WITH_UNIT (LENGTH_MEASURE( 1.000000000000000082E-05 ), #2863, 'distance_accuracy_value', 'NONE');
#9682 = CIRCLE ( 'NONE', #11626, 1.000000000000000888 ) ;
#9683 = EDGE_LOOP ( 'NONE', ( #2294, #12691, #11252, #7574, #11981, #2950, #10326, #4363 ) ) ;
#9684 = DIRECTION ( 'NONE',  ( -0.000000000000000000, -0.000000000000000000, 1.000000000000000000 ) ) ;
#9685 = ORIENTED_EDGE ( 'NONE', *, *, #11666, .T. ) ;
#9686 = ORIENTED_EDGE ( 'NONE', *, *, #13099, .F. ) ;
#9687 = DIRECTION ( 'NONE',  ( 0.000000000000000000, 0.000000000000000000, -1.000000000000000000 ) ) ;
#9688 = DIRECTION ( 'NONE',  ( 0.5394184268574520047, -0.8420378618367654333, 0.000000000000000000 ) ) ;
#9689 = B_SPLINE_CURVE_WITH_KNOTS ( 'NONE', 3,
 ( #10057, #8293, #9601, #3587 ),
 .UNSPECIFIED., .F., .F.,
 ( 4, 4 ),
 ( 0.000000000000000000, 0.006642648484603335887 ),
 .UNSPECIFIED. ) ;
#9690 = FACE_OUTER_BOUND ( 'NONE', #6350, .T. ) ;
#9691 = ORIENTED_EDGE ( 'NONE', *, *, #2750, .T. ) ;
#9692 = EDGE_CURVE ( 'NONE', #11155, #2180, #9125, .T. ) ;
#9693 = ORIENTED_EDGE ( 'NONE', *, *, #55, .T. ) ;
#9694 = AXIS2_PLACEMENT_3D ( 'NONE', #9908, #14587, #4036 ) ;
#9695 = CARTESIAN_POINT ( 'NONE',  ( 8.201103799357262858, -57.48563641131178770, 1.816685854991388682 ) ) ;
#9696 = VECTOR ( 'NONE', #11681, 1000.000000000000000 ) ;
#9697 = CARTESIAN_POINT ( 'NONE',  ( 65.00000000000001421, -85.24929059928631148, 17.47499999999999787 ) ) ;
#9698 = DIRECTION ( 'NONE',  ( 0.000000000000000000, 0.000000000000000000, 1.000000000000000000 ) ) ;
#9699 = ORIENTED_EDGE ( 'NONE', *, *, #3344, .F. ) ;
#9700 = VERTEX_POINT ( 'NONE', #659 ) ;
#9701 = DIRECTION ( 'NONE',  ( 0.000000000000000000, 1.000000000000000000, 0.000000000000000000 ) ) ;
#9702 = ORIENTED_EDGE ( 'NONE', *, *, #14499, .T. ) ;
#9703 = CARTESIAN_POINT ( 'NONE',  ( 13.90935834228072743, -66.06148843087628109, 4.401172203687842455 ) ) ;
#9704 = ORIENTED_EDGE ( 'NONE', *, *, #6908, .F. ) ;
#9705 = ORIENTED_EDGE ( 'NONE', *, *, #6853, .T. ) ;
#9706 = PLANE ( 'NONE',  #8281 ) ;
#9707 = DIRECTION ( 'NONE',  ( -0.5006040828730976555, 0.8656763553492637930, 0.000000000000000000 ) ) ;
#9708 = VERTEX_POINT ( 'NONE', #3059 ) ;
#9709 = EDGE_CURVE ( 'NONE', #8896, #5290, #9252, .T. ) ;
#9710 = CARTESIAN_POINT ( 'NONE',  ( 29.05371116072213056, -64.60713873539394569, -3.212402267258252397 ) ) ;
#9711 = DIRECTION ( 'NONE',  ( -0.000000000000000000, 1.000000000000000000, 1.445602896647339163E-16 ) ) ;
#9712 = VERTEX_POINT ( 'NONE', #11274 ) ;
#9713 = PLANE ( 'NONE',  #9022 ) ;
#9714 = DIRECTION ( 'NONE',  ( 0.7398406760702315177, 0.6727821148276332819, 8.214872995831076759E-16 ) ) ;
#9715 = B_SPLINE_CURVE_WITH_KNOTS ( 'NONE', 3,
 ( #6253, #1313, #6312, #13021, #4932, #7394, #11007, #11926, #2697, #14474 ),
 .UNSPECIFIED., .F., .F.,
 ( 4, 2, 2, 2, 4 ),
 ( 0.000000000000000000, 0.0004605959310618659556, 0.0009211918621237319112, 0.001381787793185597921, 0.001842383724247463822 ),
 .UNSPECIFIED. ) ;
#9716 = DIRECTION ( 'NONE',  ( 0.000000000000000000, -0.000000000000000000, -1.000000000000000000 ) ) ;
#9717 = ORIENTED_EDGE ( 'NONE', *, *, #335, .F. ) ;
#9718 = CARTESIAN_POINT ( 'NONE',  ( -22.42998452855183444, 4.960558937058127782, 48.26605223428308733 ) ) ;
#9719 = ADVANCED_FACE ( 'NONE', ( #5443 ), #10138, .T. ) ;
#9720 = EDGE_CURVE ( 'NONE', #3629, #14995, #1633, .T. ) ;
#9721 = EDGE_LOOP ( 'NONE', ( #5944, #2533, #739, #5769 ) ) ;
#9722 = DIRECTION ( 'NONE',  ( 0.8746197071345573892, -0.4848096202550657430, 0.000000000000000000 ) ) ;
#9723 = ORIENTED_EDGE ( 'NONE', *, *, #9418, .F. ) ;
#9724 = B_SPLINE_CURVE_WITH_KNOTS ( 'NONE', 3,
 ( #12299, #1755, #2912, #13450 ),
 .UNSPECIFIED., .F., .F.,
 ( 4, 4 ),
 ( 0.000000000000000000, 0.006683255761480933789 ),
 .UNSPECIFIED. ) ;
#9725 = DIRECTION ( 'NONE',  ( -0.3020115420618222357, 0.1674077314120182292, -0.9384901064608630605 ) ) ;
#9726 = LINE ( 'NONE', #9869, #1285 ) ;
#9727 = EDGE_CURVE ( 'NONE', #12771, #2922, #10234, .T. ) ;
#9728 = FACE_OUTER_BOUND ( 'NONE', #5370, .T. ) ;
#9729 = DIRECTION ( 'NONE',  ( -0.000000000000000000, -0.000000000000000000, -1.000000000000000000 ) ) ;
#9730 = CARTESIAN_POINT ( 'NONE',  ( 80.00000000000001421, -74.24929059928631148, -8.000000000000001776 ) ) ;
#9731 = DIRECTION ( 'NONE',  ( -0.000000000000000000, 0.000000000000000000, -1.000000000000000000 ) ) ;
#9732 = EDGE_CURVE ( 'NONE', #4371, #3752, #10294, .T. ) ;
#9733 = CARTESIAN_POINT ( 'NONE',  ( 58.00000000000000711, 7.750709400713694741, 38.00000000000012079 ) ) ;
#9734 = CARTESIAN_POINT ( 'NONE',  ( -16.99999999999998579, -2.249290599286303927, -50.00000000000012079 ) ) ;
#9735 = CARTESIAN_POINT ( 'NONE',  ( 32.05873099921245029, -53.19870790407433248, -3.318692829849283932 ) ) ;
#9736 = CARTESIAN_POINT ( 'NONE',  ( 20.86173033120691045, -52.24929059928630437, 0.000000000000000000 ) ) ;
#9737 = EDGE_LOOP ( 'NONE', ( #2424, #8323, #3085, #1537 ) ) ;
#9738 = LINE ( 'NONE', #7945, #10129 ) ;
#9739 = CARTESIAN_POINT ( 'NONE',  ( 32.52281604437752804, -59.06479067038041819, -2.757123406423251044 ) ) ;
#9740 = DIRECTION ( 'NONE',  ( -0.000000000000000000, -0.000000000000000000, -1.000000000000000000 ) ) ;
#9741 = EDGE_CURVE ( 'NONE', #3172, #6140, #11672, .T. ) ;
#9742 = CARTESIAN_POINT ( 'NONE',  ( 76.63070922904937277, -6.859691020777845871, 75.19766410831374515 ) ) ;
#9743 = LINE ( 'NONE', #2804, #1766 ) ;
#9744 = CARTESIAN_POINT ( 'NONE',  ( 80.18290120114222930, 25.52935533987996664, 84.20452624982236500 ) ) ;
#9745 = DIRECTION ( 'NONE',  ( -0.000000000000000000, 1.000000000000000000, -0.000000000000000000 ) ) ;
#9746 = AXIS2_PLACEMENT_3D ( 'NONE', #2172, #11549, #15029 ) ;
#9747 = ORIENTED_EDGE ( 'NONE', *, *, #12708, .T. ) ;
#9748 = CARTESIAN_POINT ( 'NONE',  ( 58.00000000000000711, -2.249290599286311032, -38.00000000000012079 ) ) ;
#9749 = ORIENTED_EDGE ( 'NONE', *, *, #5658, .F. ) ;
#9750 = LINE ( 'NONE', #9896, #5699 ) ;
#9751 = CARTESIAN_POINT ( 'NONE',  ( 29.35555050496136431, -56.52532528994181860, 2.500000000000000000 ) ) ;
#9752 = ORIENTED_EDGE ( 'NONE', *, *, #7758, .T. ) ;
#9754 = ORIENTED_EDGE ( 'NONE', *, *, #1430, .T. ) ;
#9753 = FACE_OUTER_BOUND ( 'NONE', #14255, .T. ) ;
#9755 = CARTESIAN_POINT ( 'NONE',  ( 58.00000000000000711, 10.75070940071368852, 139.1143251403882459 ) ) ;
#9756 = EDGE_CURVE ( 'NONE', #13017, #11141, #5600, .T. ) ;
#9757 = ADVANCED_FACE ( 'NONE', ( #12841 ), #3602, .F. ) ;
#9758 = AXIS2_PLACEMENT_3D ( 'NONE', #6512, #13670, #5214 ) ;
#9759 = CARTESIAN_POINT ( 'NONE',  ( -22.16581936427349575, -2.249290599286304371, -57.50000000000012079 ) ) ;
#9760 = ORIENTED_EDGE ( 'NONE', *, *, #6868, .T. ) ;
#9761 = DIRECTION ( 'NONE',  ( 1.000000000000000000, 0.000000000000000000, 0.000000000000000000 ) ) ;
#9762 = FACE_OUTER_BOUND ( 'NONE', #11927, .T. ) ;
#9763 = CARTESIAN_POINT ( 'NONE',  ( 9.573486461617509491, -58.98766849246937483, -1.832439066040240983 ) ) ;
#9764 = AXIS2_PLACEMENT_3D ( 'NONE', #6300, #8678, #10846 ) ;
#9765 = ORIENTED_EDGE ( 'NONE', *, *, #3328, .T. ) ;
#9766 = AXIS2_PLACEMENT_3D ( 'NONE', #6283, #10974, #429 ) ;
#9767 = CARTESIAN_POINT ( 'NONE',  ( 64.16994054879148734, -11.91212264076314575, 75.71502901994244894 ) ) ;
#9768 = ORIENTED_EDGE ( 'NONE', *, *, #9344, .T. ) ;
#9769 = CARTESIAN_POINT ( 'NONE',  ( -21.99701278316016584, 5.237925250804929433, 48.44214661496815211 ) ) ;
#9770 = EDGE_LOOP ( 'NONE', ( #2908, #13650, #9147, #2247, #14740, #8614, #4298 ) ) ;
#9771 = CARTESIAN_POINT ( 'NONE',  ( 12.03298173962126327, -53.28399145779480506, 4.141535524925031631 ) ) ;
#9772 = EDGE_CURVE ( 'NONE', #4994, #7307, #888, .T. ) ;
#9773 = ADVANCED_FACE ( 'NONE', ( #7983 ), #9371, .T. ) ;
#9774 = ORIENTED_EDGE ( 'NONE', *, *, #7498, .F. ) ;
#9775 = AXIS2_PLACEMENT_3D ( 'NONE', #4634, #10413, #7017 ) ;
#9776 = DIRECTION ( 'NONE',  ( 1.000000000000000000, -2.602085213965208275E-15, 0.000000000000000000 ) ) ;
#9777 = FACE_OUTER_BOUND ( 'NONE', #4330, .T. ) ;
#9778 = ORIENTED_EDGE ( 'NONE', *, *, #3068, .T. ) ;
#9779 = DIRECTION ( 'NONE',  ( 0.000000000000000000, -1.445602896647339163E-16, 1.000000000000000000 ) ) ;
#9780 = ORIENTED_EDGE ( 'NONE', *, *, #7759, .T. ) ;
#9781 = CARTESIAN_POINT ( 'NONE',  ( 80.18290120114222930, 23.25070940071369208, 84.20452624982236500 ) ) ;
#9782 = FACE_OUTER_BOUND ( 'NONE', #13588, .T. ) ;
#9783 = DIRECTION ( 'NONE',  ( -0.000000000000000000, 1.000000000000000000, -0.000000000000000000 ) ) ;
#9784 = CIRCLE ( 'NONE', #4867, 0.9999999999999957812 ) ;
#9785 = AXIS2_PLACEMENT_3D ( 'NONE', #1242, #11077, #1476 ) ;
#9786 = ORIENTED_EDGE ( 'NONE', *, *, #4897, .F. ) ;
#9787 = CARTESIAN_POINT ( 'NONE',  ( -23.95855436784179560, 3.468451880982295954, 47.93156476714377590 ) ) ;
#9788 = CONICAL_SURFACE ( 'NONE', #9536, 2.524999999999999467, 0.7853981633973787790 ) ;
#9789 = ORIENTED_EDGE ( 'NONE', *, *, #12920, .F. ) ;
#9790 = CIRCLE ( 'NONE', #13459, 1.000000000000000888 ) ;
#9791 = ORIENTED_EDGE ( 'NONE', *, *, #609, .F. ) ;
#9792 = FACE_OUTER_BOUND ( 'NONE', #5654, .T. ) ;
#9793 = ORIENTED_EDGE ( 'NONE', *, *, #4861, .T. ) ;
#9794 = CONTEXT_DEPENDENT_SHAPE_REPRESENTATION ( #1428, #12591 ) ;
#9795 = FACE_OUTER_BOUND ( 'NONE', #8873, .T. ) ;
#9796 = ADVANCED_FACE ( 'NONE', ( #2124 ), #2210, .F. ) ;
#9797 = DIRECTION ( 'NONE',  ( 1.000000000000000000, 0.000000000000000000, 0.000000000000000000 ) ) ;
#9798 = AXIS2_PLACEMENT_3D ( 'NONE', #11625, #1081, #5792 ) ;
#9799 = LINE ( 'NONE', #537, #1121 ) ;
#9800 = CARTESIAN_POINT ( 'NONE',  ( 17.78537369493595932, -66.03679020171973946, 6.288305159853288195 ) ) ;
#9801 = ADVANCED_FACE ( 'NONE', ( #4672 ), #159, .T. ) ;
#9802 = VECTOR ( 'NONE', #257, 1000.000000000000000 ) ;
#9803 = ADVANCED_FACE ( 'NONE', ( #4353 ), #11425, .T. ) ;
#9804 = CARTESIAN_POINT ( 'NONE',  ( 31.72322230991231962, -61.42570632716525125, 2.132522520905362651 ) ) ;
#9805 = LINE ( 'NONE', #2635, #3912 ) ;
#9806 = CARTESIAN_POINT ( 'NONE',  ( 33.04176068768711616, -54.35228707169699192, 2.121495901600882750 ) ) ;
#9807 = FACE_BOUND ( 'NONE', #5120, .T. ) ;
#9808 = AXIS2_PLACEMENT_3D ( 'NONE', #7326, #3852, #13326 ) ;
#9809 = EDGE_CURVE ( 'NONE', #3269, #10461, #12763, .T. ) ;
#9810 = EDGE_CURVE ( 'NONE', #12141, #14247, #11957, .T. ) ;
#9811 = CARTESIAN_POINT ( 'NONE',  ( -9.084028622109864060, 2.040253803610913685, 48.06338840812200175 ) ) ;
#9812 = ORIENTED_EDGE ( 'NONE', *, *, #242, .F. ) ;
#9813 = CARTESIAN_POINT ( 'NONE',  ( -24.55590860040002710, -7.139109479066534369, -48.24517880332174968 ) ) ;
#9814 = DIRECTION ( 'NONE',  ( -0.000000000000000000, 0.000000000000000000, 1.000000000000000000 ) ) ;
#9815 = EDGE_CURVE ( 'NONE', #14996, #14228, #15138, .T. ) ;
#9816 = CARTESIAN_POINT ( 'NONE',  ( -26.99999999999998934, -2.249290599286302150, -32.99999999999987921 ) ) ;
#9817 = CARTESIAN_POINT ( 'NONE',  ( 64.12538157620423362, -11.94043129933760206, 72.93296134066703473 ) ) ;
#9818 = EDGE_CURVE ( 'NONE', #7033, #6024, #10600, .T. ) ;
#9819 = ADVANCED_FACE ( 'NONE', ( #7056 ), #4516, .T. ) ;
#9820 = DIRECTION ( 'NONE',  ( 1.000000000000000000, 0.000000000000000000, 0.000000000000000000 ) ) ;
#9821 = CARTESIAN_POINT ( 'NONE',  ( 9.074528850133887659, -58.48798588983495250, -2.754379989677188334 ) ) ;
#9822 = ORIENTED_EDGE ( 'NONE', *, *, #7544, .F. ) ;
#9823 = CARTESIAN_POINT ( 'NONE',  ( 32.86505965715682720, -57.78267463900354528, -2.727521282214311782 ) ) ;
#9824 = ORIENTED_EDGE ( 'NONE', *, *, #476, .T. ) ;
#9825 = CARTESIAN_POINT ( 'NONE',  ( 80.00000000000001421, -72.24929059928631148, 32.99999999999999289 ) ) ;
#9826 = DIRECTION ( 'NONE',  ( 0.000000000000000000, 0.000000000000000000, -1.000000000000000000 ) ) ;
#9827 = ORIENTED_EDGE ( 'NONE', *, *, #10832, .T. ) ;
#9828 = CARTESIAN_POINT ( 'NONE',  ( 63.36453054171181520, -0.8129776999179910701, 60.61639468829817190 ) ) ;
#9829 = DIRECTION ( 'NONE',  ( 1.000000000000000000, 0.000000000000000000, 0.000000000000000000 ) ) ;
#9830 = ORIENTED_EDGE ( 'NONE', *, *, #3711, .T. ) ;
#9831 = VECTOR ( 'NONE', #5557, 1000.000000000000000 ) ;
#9832 = CARTESIAN_POINT ( 'NONE',  ( 31.10334365618823327, -60.64100864355887666, -2.132522520905395513 ) ) ;
#9833 = EDGE_LOOP ( 'NONE', ( #14848, #9546, #2417, #574 ) ) ;
#9834 = PLANE ( 'NONE',  #2408 ) ;
#9835 = EDGE_CURVE ( 'NONE', #13383, #1549, #9058, .T. ) ;
#9836 = DIRECTION ( 'NONE',  ( 0.000000000000000000, 0.000000000000000000, 1.000000000000000000 ) ) ;
#9837 = EDGE_CURVE ( 'NONE', #1708, #9017, #3112, .T. ) ;
#9838 = CARTESIAN_POINT ( 'NONE',  ( -3.999999999999976019, -69.24929059928631148, 33.00000000000000711 ) ) ;
#9839 = AXIS2_PLACEMENT_3D ( 'NONE', #14643, #13569, #7501 ) ;
#9840 = ORIENTED_EDGE ( 'NONE', *, *, #5988, .F. ) ;
#9841 = ORIENTED_EDGE ( 'NONE', *, *, #1177, .T. ) ;
#9842 = PLANE ( 'NONE',  #12704 ) ;
#9843 = VERTEX_POINT ( 'NONE', #3741 ) ;
#9844 = CYLINDRICAL_SURFACE ( 'NONE', #2977, 0.7892041907098261699 ) ;
#9845 = ORIENTED_EDGE ( 'NONE', *, *, #525, .F. ) ;
#9846 = CARTESIAN_POINT ( 'NONE',  ( 108.0866310645538562, 23.25070940071369563, -33.00000000000012790 ) ) ;
#9847 = VERTEX_POINT ( 'NONE', #137 ) ;
#9848 = CARTESIAN_POINT ( 'NONE',  ( -2.016677571526633510E-15, 23.25070940071368497, 139.1143251403882459 ) ) ;
#9849 = DIRECTION ( 'NONE',  ( 0.000000000000000000, 0.000000000000000000, 1.000000000000000000 ) ) ;
#9850 = EDGE_LOOP ( 'NONE', ( #2494, #8153, #12047, #13823 ) ) ;
#9851 = VECTOR ( 'NONE', #8858, 1000.000000000000000 ) ;
#9852 = CARTESIAN_POINT ( 'NONE',  ( 27.94380378979190382, -67.87804980504907348, -4.252496648647420052 ) ) ;
#9853 = ORIENTED_EDGE ( 'NONE', *, *, #5612, .T. ) ;
#9854 = ADVANCED_FACE ( 'NONE', ( #13138 ), #1279, .F. ) ;
#9855 = CARTESIAN_POINT ( 'NONE',  ( 62.00000000000001421, -2.249290599286310588, 33.00000000000012790 ) ) ;
#9856 = DIRECTION ( 'NONE',  ( -0.000000000000000000, 0.000000000000000000, 1.000000000000000000 ) ) ;
#9857 = ADVANCED_FACE ( 'NONE', ( #5052 ), #8299, .T. ) ;
#9858 = PRODUCT_DEFINITION ( 'UNKNOWN', '', #15181, #5987 ) ;
#9859 = CARTESIAN_POINT ( 'NONE',  ( 100.1541764164548880, 23.25070940071369208, 139.1143251403882459 ) ) ;
#9860 = EDGE_LOOP ( 'NONE', ( #11905, #12817, #9760, #13945 ) ) ;
#9861 = LINE ( 'NONE', #14685, #14694 ) ;
#9862 = ORIENTED_EDGE ( 'NONE', *, *, #13784, .F. ) ;
#9863 = EDGE_LOOP ( 'NONE', ( #14305, #3840, #3648, #11221 ) ) ;
#9864 = ORIENTED_EDGE ( 'NONE', *, *, #3568, .T. ) ;
#9865 = LINE ( 'NONE', #12006, #7927 ) ;
#9866 = AXIS2_PLACEMENT_3D ( 'NONE', #10764, #5928, #4835 ) ;
#9867 = SHAPE_DEFINITION_REPRESENTATION ( #5233, #15125 ) ;
#9868 = PLANE ( 'NONE',  #3874 ) ;
#9869 = CARTESIAN_POINT ( 'NONE',  ( 80.00000000000001421, -87.24929059928631148, -35.00000000000000000 ) ) ;
#9870 = CARTESIAN_POINT ( 'NONE',  ( 80.00000000000001421, -85.24929059928631148, -6.000000000000001776 ) ) ;
#9871 = VECTOR ( 'NONE', #1348, 1000.000000000000000 ) ;
#9872 = CARTESIAN_POINT ( 'NONE',  ( 13.46770580362635350, -61.89598878762631529, 4.173736770066597046 ) ) ;
#9873 = CARTESIAN_POINT ( 'NONE',  ( -9.871163676013017252, -8.117995983050501962, -48.08465436988272046 ) ) ;
#9874 = DIRECTION ( 'NONE',  ( 0.7392394270158823000, -0.6734426995262700055, 0.000000000000000000 ) ) ;
#9875 = LINE ( 'NONE', #14704, #10812 ) ;
#9876 = AXIS2_PLACEMENT_3D ( 'NONE', #3182, #6643, #11328 ) ;
#9877 = CIRCLE ( 'NONE', #4952, 0.7892041907098278353 ) ;
#9878 = AXIS2_PLACEMENT_3D ( 'NONE', #1091, #8024, #7175 ) ;
#9879 = DIRECTION ( 'NONE',  ( 0.000000000000000000, 1.000000000000000000, -0.000000000000000000 ) ) ;
#9880 = ORIENTED_EDGE ( 'NONE', *, *, #1566, .F. ) ;
#9881 = DIRECTION ( 'NONE',  ( -0.8746197071345571672, 0.4848096202550660205, 0.000000000000000000 ) ) ;
#9882 = DIRECTION ( 'NONE',  ( 0.000000000000000000, 1.000000000000000000, 0.000000000000000000 ) ) ;
#9883 = AXIS2_PLACEMENT_3D ( 'NONE', #3166, #7716, #12403 ) ;
#9884 = CARTESIAN_POINT ( 'NONE',  ( 112.9262740340969060, 21.75070940071369918, 139.1143251403882459 ) ) ;
#9885 = AXIS2_PLACEMENT_3D ( 'NONE', #8682, #12375, #14531 ) ;
#9886 = EDGE_CURVE ( 'NONE', #1292, #8692, #14192, .T. ) ;
#9887 = CIRCLE ( 'NONE', #3241, 0.7892041907098262810 ) ;
#9888 = DIRECTION ( 'NONE',  ( 1.000000000000000000, 0.000000000000000000, 0.000000000000000000 ) ) ;
#9889 = CARTESIAN_POINT ( 'NONE',  ( 28.30879605499156071, -66.31562986446991204, -3.513916789801494467 ) ) ;
#9890 = VERTEX_POINT ( 'NONE', #9529 ) ;
#9891 = FACE_OUTER_BOUND ( 'NONE', #3309, .T. ) ;
#9892 = VECTOR ( 'NONE', #12271, 1000.000000000000000 ) ;
#9893 = CIRCLE ( 'NONE', #5975, 3.999999999999994227 ) ;
#9894 = ORIENTED_EDGE ( 'NONE', *, *, #4862, .T. ) ;
#9895 = EDGE_CURVE ( 'NONE', #14607, #6894, #12206, .T. ) ;
#9896 = CARTESIAN_POINT ( 'NONE',  ( 80.00000000000001421, -72.24929059928631148, -32.99999999999999289 ) ) ;
#9897 = CARTESIAN_POINT ( 'NONE',  ( 20.86173033120691045, -85.24929059928631148, 0.000000000000000000 ) ) ;
#9898 = AXIS2_PLACEMENT_3D ( 'NONE', #8542, #13242, #2687 ) ;
#9899 = EDGE_CURVE ( 'NONE', #6894, #14607, #2865, .T. ) ;
#9900 = ORIENTED_EDGE ( 'NONE', *, *, #4034, .T. ) ;
#9901 = LINE ( 'NONE', #7578, #1038 ) ;
#9902 = CARTESIAN_POINT ( 'NONE',  ( 56.59738969056744651, 0.000000000000000000, 139.1143251403882459 ) ) ;
#9903 = AXIS2_PLACEMENT_3D ( 'NONE', #3687, #4921, #9311 ) ;
#9904 = FACE_OUTER_BOUND ( 'NONE', #4893, .T. ) ;
#9905 = VECTOR ( 'NONE', #1947, 1000.000000000000000 ) ;
#9906 = CARTESIAN_POINT ( 'NONE',  ( 33.53865989972762662, 5.593081289880174722, 89.15517579724127017 ) ) ;
#9907 = AXIS2_PLACEMENT_3D ( 'NONE', #15224, #1286, #7990 ) ;
#9908 = CARTESIAN_POINT ( 'NONE',  ( 72.26742264675378635, -14.73126838498886571, 75.19766410831374515 ) ) ;
#9909 = CARTESIAN_POINT ( 'NONE',  ( 62.67308791069655882, 29.52935533987996664, -33.00000000000013500 ) ) ;
#9910 = AXIS2_PLACEMENT_3D ( 'NONE', #6144, #10827, #288 ) ;
#9911 = VERTEX_POINT ( 'NONE', #2440 ) ;
#9912 = ORIENTED_EDGE ( 'NONE', *, *, #6225, .F. ) ;
#9913 = DIRECTION ( 'NONE',  ( -1.000000000000000000, 0.000000000000000000, 0.000000000000000000 ) ) ;
#9914 = ORIENTED_EDGE ( 'NONE', *, *, #12736, .T. ) ;
#9915 =( BOUNDED_SURFACE ( )  B_SPLINE_SURFACE ( 3, 2, ( 
 ( #5914, #5994, #8298 ),
 ( #9604, #2518, #13136 ),
 ( #136, #4671, #2439 ),
 ( #3739, #6139, #1207 ),
 ( #10596, #6983, #14371 ),
 ( #10824, #283, #7135 ),
 ( #12840, #7281, #2289 ),
 ( #11899, #12918, #61 ),
 ( #4978, #9370, #4823 ),
 ( #4754, #8225, #9450 ),
 ( #2362, #14142, #9528 ),
 ( #3590, #14218, #6059 ),
 ( #3669, #8371, #13062 ),
 ( #1358, #10751, #11969 ) ),
 .UNSPECIFIED., .F., .F., .F. ) 
 B_SPLINE_SURFACE_WITH_KNOTS ( ( 4, 2, 2, 2, 2, 2, 4 ),
 ( 3, 3 ),
 ( 0.001231944704344891230, 0.001640530120327067607, 0.002049115536309244201, 0.002866286368273596955, 0.003274871784255773549, 0.003683457200237949709, 0.004500628032202302897 ),
 ( 0.000000000000000000, 1.000000000000000000 ),
 .UNSPECIFIED. ) 
 GEOMETRIC_REPRESENTATION_ITEM ( )  RATIONAL_B_SPLINE_SURFACE ( (
 ( 1.000000000000000000, 0.8606282562001377201, 1.000000000000000000),
 ( 1.000000000000000000, 0.8606242962982729727, 1.000000000000000000),
 ( 1.000000000000000000, 0.8593044206444694355, 1.000000000000000000),
 ( 1.000000000000000000, 0.8542070032136860336, 1.000000000000000000),
 ( 1.000000000000000000, 0.8503651661365319026, 1.000000000000000000),
 ( 1.000000000000000000, 0.8359148296419828261, 1.000000000000000000),
 ( 1.000000000000000000, 0.8221039232031693844, 1.000000000000000000),
 ( 1.000000000000000000, 0.7986554744404532613, 1.000000000000000000),
 ( 1.000000000000000000, 0.7902603328757243917, 1.000000000000000000),
 ( 1.000000000000000000, 0.7732499594492155959, 1.000000000000000000),
 ( 1.000000000000000000, 0.7646145331269290635, 1.000000000000000000),
 ( 1.000000000000000000, 0.7387090984033097829, 1.000000000000000000),
 ( 1.000000000000000000, 0.7216377403000998614, 1.000000000000000000),
 ( 1.000000000000000000, 0.7071067811865457964, 1.000000000000000000) ) ) 
 REPRESENTATION_ITEM ( '' )  SURFACE ( )  );
#9916 = CARTESIAN_POINT ( 'NONE',  ( 29.93258319667773293, -53.28557432868839072, -4.055360768045983555 ) ) ;
#9917 = VERTEX_POINT ( 'NONE', #8372 ) ;
#9918 = FACE_OUTER_BOUND ( 'NONE', #4981, .T. ) ;
#9919 = DIRECTION ( 'NONE',  ( -1.000000000000000000, 0.000000000000000000, 0.000000000000000000 ) ) ;
#9920 = EDGE_LOOP ( 'NONE', ( #1712, #11182, #13075, #9095 ) ) ;
#9921 = AXIS2_PLACEMENT_3D ( 'NONE', #290, #6226, #3674 ) ;
#9922 = CARTESIAN_POINT ( 'NONE',  ( 80.00000000000001421, -85.24929059928629727, 32.00000000000000000 ) ) ;
#9923 = CARTESIAN_POINT ( 'NONE',  ( -3.535822565187055400, 6.114368811827579187, 57.50000000000012079 ) ) ;
#9924 = ORIENTED_EDGE ( 'NONE', *, *, #10546, .F. ) ;
#9925 = ADVANCED_FACE ( 'NONE', ( #13214 ), #7361, .F. ) ;
#9926 = AXIS2_PLACEMENT_3D ( 'NONE', #5377, #13608, #2773 ) ;
#9927 = DIRECTION ( 'NONE',  ( 0.8420378618367644341, 0.5394184268574535590, 0.000000000000000000 ) ) ;
#9928 = VERTEX_POINT ( 'NONE', #5995 ) ;
#9929 = CARTESIAN_POINT ( 'NONE',  ( 63.04142083571589694, -2.691337429055927988, 62.84860122826521689 ) ) ;
#9930 = DIRECTION ( 'NONE',  ( -0.8746197071345572782, 0.4848096202550659650, 0.000000000000000000 ) ) ;
#9931 = DIRECTION ( 'NONE',  ( -1.000000000000000000, 0.000000000000000000, 0.000000000000000000 ) ) ;
#9932 = ORIENTED_EDGE ( 'NONE', *, *, #8499, .F. ) ;
#9933 = DIRECTION ( 'NONE',  ( 0.000000000000000000, 1.000000000000000000, 0.000000000000000000 ) ) ;
#9934 = ORIENTED_EDGE ( 'NONE', *, *, #13734, .F. ) ;
#9935 = CIRCLE ( 'NONE', #7475, 0.7892041907098261699 ) ;
#9936 = ORIENTED_EDGE ( 'NONE', *, *, #6904, .F. ) ;
#9937 = ORIENTED_EDGE ( 'NONE', *, *, #5554, .T. ) ;
#9938 = DIRECTION ( 'NONE',  ( 0.000000000000000000, 1.000000000000000000, 0.000000000000000000 ) ) ;
#9939 = PRODUCT_CONTEXT ( 'NONE', #12966, 'mechanical' ) ;
#9940 = DIRECTION ( 'NONE',  ( 0.000000000000000000, -3.469446951953611033E-15, 1.000000000000000000 ) ) ;
#9941 = PLANE ( 'NONE',  #13332 ) ;
#9942 = ADVANCED_FACE ( 'NONE', ( #9607 ), #6072, .T. ) ;
#9943 = EDGE_CURVE ( 'NONE', #5460, #12879, #2626, .T. ) ;
#9944 = DIRECTION ( 'NONE',  ( 0.8656763553492639041, 0.5006040828730973224, -0.000000000000000000 ) ) ;
#9945 = ORIENTED_EDGE ( 'NONE', *, *, #4519, .F. ) ;
#9946 = DIRECTION ( 'NONE',  ( -0.000000000000000000, -0.000000000000000000, 1.000000000000000000 ) ) ;
#9947 = DIRECTION ( 'NONE',  ( 0.000000000000000000, 0.000000000000000000, 1.000000000000000000 ) ) ;
#9948 = LINE ( 'NONE', #1922, #4499 ) ;
#9949 = CARTESIAN_POINT ( 'NONE',  ( 13.12221348233057938, -65.57050171853553877, -4.044987206835411797 ) ) ;
#9950 = ORIENTED_EDGE ( 'NONE', *, *, #6357, .T. ) ;
#9951 = CARTESIAN_POINT ( 'NONE',  ( 32.95695892024548357, -57.08411837894883689, 2.747858231243594407 ) ) ;
#9952 = CARTESIAN_POINT ( 'NONE',  ( -8.650962968042231083, 2.291620771759304898, 48.06291368403883268 ) ) ;
#9953 = ORIENTED_EDGE ( 'NONE', *, *, #12230, .T. ) ;
#9954 = FILL_AREA_STYLE ('',( #6200 ) ) ;
#9955 = DIRECTION ( 'NONE',  ( -0.000000000000000000, -0.000000000000000000, -1.000000000000000000 ) ) ;
#9956 = EDGE_CURVE ( 'NONE', #11167, #3925, #7282, .T. ) ;
#9957 = CARTESIAN_POINT ( 'NONE',  ( -16.99999999999998579, -2.249290599286303927, 57.50000000000012079 ) ) ;
#9958 = ORIENTED_EDGE ( 'NONE', *, *, #9193, .F. ) ;
#9959 = DIRECTION ( 'NONE',  ( 0.3020115420618248447, -0.1674077314120183957, 0.9384901064608620613 ) ) ;
#9960 = CARTESIAN_POINT ( 'NONE',  ( 62.67308791069655882, 29.52935533987996664, 33.00000000000014211 ) ) ;
#9961 = DIRECTION ( 'NONE',  ( -0.000000000000000000, -0.000000000000000000, 1.000000000000000000 ) ) ;
#9962 = LINE ( 'NONE', #6558, #2980 ) ;
#9963 = ORIENTED_EDGE ( 'NONE', *, *, #13035, .T. ) ;
#9964 = CARTESIAN_POINT ( 'NONE',  ( 24.14199725330118440, -70.03159917004853696, -6.184016381205399426 ) ) ;
#9965 = ORIENTED_EDGE ( 'NONE', *, *, #13939, .F. ) ;
#9966 = DIRECTION ( 'NONE',  ( -8.897452667106849240E-15, 0.000000000000000000, -1.000000000000000000 ) ) ;
#9967 = ORIENTED_EDGE ( 'NONE', *, *, #9676, .T. ) ;
#9968 = DIRECTION ( 'NONE',  ( -1.000000000000000000, 0.000000000000000000, 0.000000000000000000 ) ) ;
#9969 = CARTESIAN_POINT ( 'NONE',  ( 18.03113812440135888, -85.24929059928631148, -4.472107801411128847 ) ) ;
#9970 = LINE ( 'NONE', #6728, #8149 ) ;
#9971 = EDGE_CURVE ( 'NONE', #9847, #12140, #3615, .T. ) ;
#9972 = CARTESIAN_POINT ( 'NONE',  ( 9.438059962876366171, -53.39764053564381641, 3.230171433735036679 ) ) ;
#9973 = ADVANCED_FACE ( 'NONE', ( #1436 ), #14444, .T. ) ;
#9974 = EDGE_CURVE ( 'NONE', #7994, #355, #3360, .T. ) ;
#9975 = EDGE_CURVE ( 'NONE', #11986, #2378, #640, .T. ) ;
#9976 = CARTESIAN_POINT ( 'NONE',  ( 27.33382790127958728, -69.39711819508849544, 4.502057496415716287 ) ) ;
#9977 = CARTESIAN_POINT ( 'NONE',  ( 109.8334623555409735, 23.25070940071369563, 13.14990448602692474 ) ) ;
#9978 = ORIENTED_EDGE ( 'NONE', *, *, #6408, .T. ) ;
#9979 = FACE_OUTER_BOUND ( 'NONE', #1433, .T. ) ;
#9980 = ORIENTED_EDGE ( 'NONE', *, *, #2725, .F. ) ;
#9981 = EDGE_CURVE ( 'NONE', #77, #10905, #8517, .T. ) ;
#9982 = CYLINDRICAL_SURFACE ( 'NONE', #13306, 3.000000000000000888 ) ;
#9983 = ORIENTED_EDGE ( 'NONE', *, *, #13106, .T. ) ;
#9984 = CYLINDRICAL_SURFACE ( 'NONE', #725, 2.499999999999995115 ) ;
#9985 = AXIS2_PLACEMENT_3D ( 'NONE', #12601, #3361, #7905 ) ;
#9986 = CARTESIAN_POINT ( 'NONE',  ( 80.00000000000001421, -74.24929059928631148, -8.000000000000001776 ) ) ;
#9987 = DIRECTION ( 'NONE',  ( 1.000000000000000000, 8.673617379884035472E-17, 0.000000000000000000 ) ) ;
#9988 = LINE ( 'NONE', #2127, #13101 ) ;
#9989 = EDGE_LOOP ( 'NONE', ( #1553, #9062, #6070, #12671 ) ) ;
#9990 = CARTESIAN_POINT ( 'NONE',  ( 100.1541764164548880, 21.75070940071359615, 33.00000000000012790 ) ) ;
#9991 = EDGE_LOOP ( 'NONE', ( #8382, #1357, #5270, #11558 ) ) ;
#9992 = AXIS2_PLACEMENT_3D ( 'NONE', #1893, #11427, #6513 ) ;
#9993 = EDGE_CURVE ( 'NONE', #7396, #2597, #12131, .T. ) ;
#9994 = VECTOR ( 'NONE', #11652, 1000.000000000000000 ) ;
#9995 = CARTESIAN_POINT ( 'NONE',  ( -30.80945343098651890, -5.389243620311580329, 48.50000000000012079 ) ) ;
#9996 = DIRECTION ( 'NONE',  ( -0.000000000000000000, -0.000000000000000000, -1.000000000000000000 ) ) ;
#9997 = FACE_OUTER_BOUND ( 'NONE', #4663, .T. ) ;
#9998 = ORIENTED_EDGE ( 'NONE', *, *, #2793, .T. ) ;
#9999 = CARTESIAN_POINT ( 'NONE',  ( -6.999999999999978684, -69.24929059928631148, -115.4621125123531442 ) ) ;
#10000 = VECTOR ( 'NONE', #10837, 1000.000000000000000 ) ;
#10001 = EDGE_CURVE ( 'NONE', #72, #5415, #6500, .T. ) ;
#10002 = VERTEX_POINT ( 'NONE', #8724 ) ;
#10003 = ORIENTED_EDGE ( 'NONE', *, *, #12909, .F. ) ;
#10004 = ORIENTED_EDGE ( 'NONE', *, *, #12463, .F. ) ;
#10005 = DIRECTION ( 'NONE',  ( -0.000000000000000000, -0.000000000000000000, -1.000000000000000000 ) ) ;
#10006 = VECTOR ( 'NONE', #10809, 1000.000000000000000 ) ;
#10007 = CARTESIAN_POINT ( 'NONE',  ( 104.9938193859979236, 21.75070940071363168, 139.1143251403882459 ) ) ;
#10008 = DIRECTION ( 'NONE',  ( 0.000000000000000000, -1.000000000000000000, 1.734723475976817547E-15 ) ) ;
#10009 = DIRECTION ( 'NONE',  ( 1.000000000000000000, 0.000000000000000000, 0.000000000000000000 ) ) ;
#10010 = ORIENTED_EDGE ( 'NONE', *, *, #1124, .T. ) ;
#10011 = CIRCLE ( 'NONE', #14669, 0.9999999999999960032 ) ;
#10012 = ADVANCED_FACE ( 'NONE', ( #5348 ), #13653, .T. ) ;
#10013 = CARTESIAN_POINT ( 'NONE',  ( 70.14667088542560691, -3.748710008331756605, 76.02364810721972788 ) ) ;
#10014 = DIRECTION ( 'NONE',  ( 0.000000000000000000, 0.000000000000000000, 1.000000000000000000 ) ) ;
#10015 = AXIS2_PLACEMENT_3D ( 'NONE', #2388, #8167, #8328 ) ;
#10016 = DIRECTION ( 'NONE',  ( -0.000000000000000000, -0.000000000000000000, -1.000000000000000000 ) ) ;
#10017 = CARTESIAN_POINT ( 'NONE',  ( 13.86584091103555494, -68.67486713609660853, -3.656664647209454166 ) ) ;
#10018 = ORIENTED_EDGE ( 'NONE', *, *, #12750, .F. ) ;
#10019 = AXIS2_PLACEMENT_3D ( 'NONE', #6860, #3091, #10180 ) ;
#10020 = CARTESIAN_POINT ( 'NONE',  ( 33.52235686305655804, -57.48563641131179480, 1.816685854991386018 ) ) ;
#10021 = ADVANCED_FACE ( 'NONE', ( #6569, #10045, #638 ), #8961, .F. ) ;
#10022 = EDGE_CURVE ( 'NONE', #3269, #12669, #10119, .T. ) ;
#10023 = CARTESIAN_POINT ( 'NONE',  ( 58.00000000000000711, -2.249290599286309256, 77.19766410831374515 ) ) ;
#10024 = ORIENTED_EDGE ( 'NONE', *, *, #12051, .F. ) ;
#10025 = CARTESIAN_POINT ( 'NONE',  ( -2.016677571526633510E-15, 23.25070940071368497, 139.1143251403882459 ) ) ;
#10026 = VECTOR ( 'NONE', #14889, 1000.000000000000000 ) ;
#10027 = SHAPE_REPRESENTATION_RELATIONSHIP ( 'NONE' , 'NONE' ,  #3114, #1700 ) ;
#10028 = FACE_OUTER_BOUND ( 'NONE', #1770, .T. ) ;
#10029 = AXIS2_PLACEMENT_3D ( 'NONE', #13874, #4483, #7874 ) ;
#10030 = DIRECTION ( 'NONE',  ( -0.8746197071345572782, 0.4848096202550659650, -0.000000000000000000 ) ) ;
#10031 = DIRECTION ( 'NONE',  ( 0.000000000000000000, 0.000000000000000000, -1.000000000000000000 ) ) ;
#10032 = CARTESIAN_POINT ( 'NONE',  ( 112.9262740340969060, 21.75070940071369918, 13.14990448602693007 ) ) ;
#10033 = CARTESIAN_POINT ( 'NONE',  ( -25.43628086306388525, -6.625164433253370788, -48.00000000000012079 ) ) ;
#10034 = CIRCLE ( 'NONE', #5363, 0.7892041907098277242 ) ;
#10035 = EDGE_CURVE ( 'NONE', #15152, #864, #11462, .T. ) ;
#10036 = ADVANCED_FACE ( 'NONE', ( #1871, #4106 ), #499, .T. ) ;
#10037 = VECTOR ( 'NONE', #273, 1000.000000000000000 ) ;
#10038 = VERTEX_POINT ( 'NONE', #9969 ) ;
#10039 = DIRECTION ( 'NONE',  ( -0.000000000000000000, -0.000000000000000000, -1.000000000000000000 ) ) ;
#10040 = ORIENTED_EDGE ( 'NONE', *, *, #2396, .F. ) ;
#10041 = CARTESIAN_POINT ( 'NONE',  ( -1.243300532054838308E-15, 10.75070940071368142, 139.1143251403882459 ) ) ;
#10042 = CARTESIAN_POINT ( 'NONE',  ( 68.00000000000000000, 2.750709400713692965, -33.00000000000012790 ) ) ;
#10043 = EDGE_LOOP ( 'NONE', ( #9139, #2910, #9306, #10024 ) ) ;
#10044 = LINE ( 'NONE', #2965, #2026 ) ;
#10045 = FACE_BOUND ( 'NONE', #15042, .T. ) ;
#10046 = CARTESIAN_POINT ( 'NONE',  ( 12.48063427020851535, -63.10178406537167461, 3.876738539648132864 ) ) ;
#10047 = CARTESIAN_POINT ( 'NONE',  ( 121.5439789431140554, -37.47229329360762762, 52.08701862022444118 ) ) ;
#10048 = FACE_OUTER_BOUND ( 'NONE', #3265, .T. ) ;
#10049 = AXIS2_PLACEMENT_3D ( 'NONE', #3987, #7234, #8684 ) ;
#10050 = CARTESIAN_POINT ( 'NONE',  ( 64.90552635791956959, 12.46743062497963450, 84.20452624982236500 ) ) ;
#10051 = CARTESIAN_POINT ( 'NONE',  ( -80.00000000000001421, -87.24929059928631148, 35.00000000000000000 ) ) ;
#10052 = ORIENTED_EDGE ( 'NONE', *, *, #6882, .T. ) ;
#10053 = CARTESIAN_POINT ( 'NONE',  ( 8.692175891108391284, -59.61959967696039797, 2.502829331402146806 ) ) ;
#10054 = ADVANCED_FACE ( 'NONE', ( #7736 ), #1660, .F. ) ;
#10055 = ORIENTED_EDGE ( 'NONE', *, *, #8455, .F. ) ;
#10056 = AXIS2_PLACEMENT_3D ( 'NONE', #15188, #1179, #8345 ) ;
#10057 = CARTESIAN_POINT ( 'NONE',  ( 18.24487436548682240, -53.24929059928630437, 6.492462156583986399 ) ) ;
#10058 = AXIS2_PLACEMENT_3D ( 'NONE', #1637, #2946, #13337 ) ;
#10059 = ORIENTED_EDGE ( 'NONE', *, *, #7721, .F. ) ;
#10060 = CARTESIAN_POINT ( 'NONE',  ( 65.00000000000001421, -85.24929059928629727, -19.99999999999999645 ) ) ;
#10061 = CARTESIAN_POINT ( 'NONE',  ( 98.40734512546775647, 21.75070940071359615, 139.1143251403882459 ) ) ;
#10062 = CARTESIAN_POINT ( 'NONE',  ( 20.86173033120691045, -53.24929059928630437, -7.000000000000000000 ) ) ;
#10063 = CARTESIAN_POINT ( 'NONE',  ( -9.037775043065352065, 2.932694901963889489, -58.00000000000012079 ) ) ;
#10064 = ORIENTED_EDGE ( 'NONE', *, *, #7971, .F. ) ;
#10065 = LINE ( 'NONE', #5530, #7915 ) ;
#10066 = VERTEX_POINT ( 'NONE', #6356 ) ;
#10067 = ADVANCED_FACE ( 'NONE', ( #13355 ), #4029, .T. ) ;
#10068 = AXIS2_PLACEMENT_3D ( 'NONE', #7988, #7497, #7065 ) ;
#10069 = EDGE_CURVE ( 'NONE', #10590, #298, #8030, .T. ) ;
#10070 = CIRCLE ( 'NONE', #10813, 1.000000000000000888 ) ;
#10071 = CARTESIAN_POINT ( 'NONE',  ( 12.05320789569630868, -52.24929059928630437, -3.114169983393155317 ) ) ;
#10072 = LINE ( 'NONE', #6675, #2042 ) ;
#10073 = DIRECTION ( 'NONE',  ( -0.000000000000000000, -0.000000000000000000, -1.000000000000000000 ) ) ;
#10074 = VERTEX_POINT ( 'NONE', #12352 ) ;
#10075 = DIRECTION ( 'NONE',  ( 0.000000000000000000, 0.000000000000000000, -1.000000000000000000 ) ) ;
#10076 = ORIENTED_EDGE ( 'NONE', *, *, #11377, .F. ) ;
#10077 = ORIENTED_EDGE ( 'NONE', *, *, #12339, .F. ) ;
#10078 = ORIENTED_EDGE ( 'NONE', *, *, #15154, .T. ) ;
#10079 = EDGE_CURVE ( 'NONE', #9444, #7182, #5254, .T. ) ;
#10080 = DIRECTION ( 'NONE',  ( 0.8746197071345571672, -0.4848096202550660205, 0.000000000000000000 ) ) ;
#10081 = AXIS2_PLACEMENT_3D ( 'NONE', #10524, #2286, #5677 ) ;
#10082 = EDGE_CURVE ( 'NONE', #10195, #14923, #2855, .T. ) ;
#10083 = FACE_OUTER_BOUND ( 'NONE', #1265, .T. ) ;
#10084 = CARTESIAN_POINT ( 'NONE',  ( -24.14404371603619381, 3.605862562765568491, -48.08251050686933326 ) ) ;
#10085 = LINE ( 'NONE', #11229, #3829 ) ;
#10086 = ORIENTED_EDGE ( 'NONE', *, *, #902, .F. ) ;
#10087 = DIRECTION ( 'NONE',  ( 0.000000000000000000, 0.000000000000000000, 1.000000000000000000 ) ) ;
#10088 = CARTESIAN_POINT ( 'NONE',  ( 65.49059688361914766, -11.82389893047565543, 72.52483798894591871 ) ) ;
#10089 = CARTESIAN_POINT ( 'NONE',  ( 69.36198185152332485, -3.785319131685315419, 77.13117128918304388 ) ) ;
#10090 = DIRECTION ( 'NONE',  ( 1.000000000000000000, 0.000000000000000000, 0.000000000000000000 ) ) ;
#10091 = AXIS2_PLACEMENT_3D ( 'NONE', #14954, #13488, #14717 ) ;
#10092 = CARTESIAN_POINT ( 'NONE',  ( 9.841896756782940514, -61.30062302791113638, -2.840369378987790405 ) ) ;
#10093 = ORIENTED_EDGE ( 'NONE', *, *, #7446, .T. ) ;
#10094 = CARTESIAN_POINT ( 'NONE',  ( 33.63312968452548546, -56.40460476644664567, 2.550424528239737754 ) ) ;
#10095 = CARTESIAN_POINT ( 'NONE',  ( -9.009135308666344599, 1.891904487837172910, 48.00342231809197102 ) ) ;
#10096 = ORIENTED_EDGE ( 'NONE', *, *, #7671, .T. ) ;
#10097 = SURFACE_STYLE_FILL_AREA ( #8780 ) ;
#10098 = PLANE ( 'NONE',  #1938 ) ;
#10099 = TOROIDAL_SURFACE ( 'NONE', #2971, 3.694885682587998765, 0.5000000000000000000 ) ;
#10100 = DIRECTION ( 'NONE',  ( 1.000000000000000000, 0.000000000000000000, 0.000000000000000000 ) ) ;
#10101 = DIRECTION ( 'NONE',  ( 0.000000000000000000, 0.000000000000000000, 1.000000000000000000 ) ) ;
#10102 = EDGE_LOOP ( 'NONE', ( #11093, #2778, #391, #9633 ) ) ;
#10103 = CARTESIAN_POINT ( 'NONE',  ( 105.5545870572953930, 23.25070940071369563, -13.14990448602692474 ) ) ;
#10104 = EDGE_CURVE ( 'NONE', #12776, #6801, #11120, .T. ) ;
#10105 = VECTOR ( 'NONE', #10612, 1000.000000000000000 ) ;
#10106 = EDGE_CURVE ( 'NONE', #5460, #170, #9264, .T. ) ;
#10107 = LINE ( 'NONE', #6866, #6142 ) ;
#10108 = CARTESIAN_POINT ( 'NONE',  ( 109.8334623555409735, 23.25070940071369563, -13.14990448602692474 ) ) ;
#10109 = CYLINDRICAL_SURFACE ( 'NONE', #1266, 0.7892041907098262810 ) ;
#10110 = CIRCLE ( 'NONE', #15024, 4.000000000000003553 ) ;
#10111 = ORIENTED_EDGE ( 'NONE', *, *, #9037, .F. ) ;
#10112 = CYLINDRICAL_SURFACE ( 'NONE', #2206, 4.000000000000000000 ) ;
#10113 = ORIENTED_EDGE ( 'NONE', *, *, #14320, .T. ) ;
#10114 = CARTESIAN_POINT ( 'NONE',  ( -2.688903428702175252E-15, 23.25070940071368142, -33.00000000000012790 ) ) ;
#10115 = CARTESIAN_POINT ( 'NONE',  ( 8.599030766203958009, -59.21224831720011395, 2.500000000000000000 ) ) ;
#10116 = VERTEX_POINT ( 'NONE', #5128 ) ;
#10117 = VECTOR ( 'NONE', #7655, 1000.000000000000000 ) ;
#10118 = CARTESIAN_POINT ( 'NONE',  ( -26.99999999999998224, -69.24929059928631148, -115.4621125123531442 ) ) ;
#10119 = LINE ( 'NONE', #4259, #14903 ) ;
#10120 = AXIS2_PLACEMENT_3D ( 'NONE', #10297, #1655, #9966 ) ;
#10121 = AXIS2_PLACEMENT_3D ( 'NONE', #3, #4926, #4694 ) ;
#10122 = CARTESIAN_POINT ( 'NONE',  ( 11.00886140161398075, -62.29356353674197067, 3.270869388470196704 ) ) ;
#10123 = EDGE_CURVE ( 'NONE', #13525, #13763, #6321, .T. ) ;
#10124 = B_SPLINE_CURVE_WITH_KNOTS ( 'NONE', 3,
 ( #2655, #11303, #9674, #8769, #10013, #6127, #10814, #762, #5475, #10165 ),
 .UNSPECIFIED., .F., .F.,
 ( 4, 2, 2, 2, 4 ),
 ( 0.000000000000000000, 0.0004549325576484883273, 0.0009098651152969778472, 0.001364797672945467421, 0.001819730230593956995 ),
 .UNSPECIFIED. ) ;
#10125 = CARTESIAN_POINT ( 'NONE',  ( 10.00262207546350979, -52.95955415863831206, 2.537984986062526538 ) ) ;
#10126 = CARTESIAN_POINT ( 'NONE',  ( 53.81626139532630049, -96.56299909827106376, -11.78977872328356646 ) ) ;
#10127 = CARTESIAN_POINT ( 'NONE',  ( 23.36173033120691400, -85.24929059928631148, 6.000000000000001776 ) ) ;
#10128 = CARTESIAN_POINT ( 'NONE',  ( 47.27423575335444639, 23.25070940071368852, 33.00000000000014211 ) ) ;
#10129 = VECTOR ( 'NONE', #9096, 1000.000000000000000 ) ;
#10130 = CIRCLE ( 'NONE', #12103, 0.4999999999999999445 ) ;
#10131 = DIRECTION ( 'NONE',  ( -0.8746197071345569451, 0.4848096202550666312, 0.000000000000000000 ) ) ;
#10132 = ORIENTED_EDGE ( 'NONE', *, *, #4232, .F. ) ;
#10133 = CARTESIAN_POINT ( 'NONE',  ( 8.701532050552359010, -59.65700314074787514, 1.835602613583684706 ) ) ;
#10134 = EDGE_LOOP ( 'NONE', ( #8379, #3482, #5261, #147 ) ) ;
#10135 = CARTESIAN_POINT ( 'NONE',  ( 32.90197589884652274, -57.33450387999030795, -2.749014434309867916 ) ) ;
#10136 = ORIENTED_EDGE ( 'NONE', *, *, #10488, .F. ) ;
#10137 = CARTESIAN_POINT ( 'NONE',  ( -1.197457146693683194, -2.220571218158922999, 57.50000000000012079 ) ) ;
#10138 = PLANE ( 'NONE',  #402 ) ;
#10139 = EDGE_CURVE ( 'NONE', #5383, #2542, #10197, .T. ) ;
#10140 = AXIS2_PLACEMENT_3D ( 'NONE', #8453, #3811, #7054 ) ;
#10141 = CARTESIAN_POINT ( 'NONE',  ( -3.190546569013415379, 0.8906624217387615339, -58.00000000000012079 ) ) ;
#10142 = CARTESIAN_POINT ( 'NONE',  ( -80.00000000000001421, -74.24929059928631148, 32.00000000000000000 ) ) ;
#10143 = ORIENTED_EDGE ( 'NONE', *, *, #5861, .T. ) ;
#10144 = CARTESIAN_POINT ( 'NONE',  ( 58.00000000000000711, -2.249290599286309256, 38.50000000000012790 ) ) ;
#10145 = ORIENTED_EDGE ( 'NONE', *, *, #9673, .F. ) ;
#10146 = CARTESIAN_POINT ( 'NONE',  ( 65.46376463298187787, -11.83285265143084963, 75.85541229843748567 ) ) ;
#10147 = CARTESIAN_POINT ( 'NONE',  ( 8.248681135559976951, -55.33002571195098795, -2.691408569076727098 ) ) ;
#10148 = CARTESIAN_POINT ( 'NONE',  ( 52.94134894379979528, -2.395505968190773327, 48.51982618741349285 ) ) ;
#10149 = DIRECTION ( 'NONE',  ( 0.8420378618367644341, 0.5394184268574535590, 0.000000000000000000 ) ) ;
#10150 = ORIENTED_EDGE ( 'NONE', *, *, #7246, .F. ) ;
#10151 = VERTEX_POINT ( 'NONE', #15045 ) ;
#10152 = CARTESIAN_POINT ( 'NONE',  ( -16.99999999999998579, -2.249290599286303927, 38.50000000000012790 ) ) ;
#10153 = EDGE_LOOP ( 'NONE', ( #5952, #9953, #10899, #11422 ) ) ;
#10154 = CARTESIAN_POINT ( 'NONE',  ( 76.78650653802468184, -6.946050879336882922, 76.19766410831374515 ) ) ;
#10155 = PRODUCT ( 'Simple Mounting Plate', 'Simple Mounting Plate', '', ( #12240 ) ) ;
#10156 = ORIENTED_EDGE ( 'NONE', *, *, #1364, .T. ) ;
#10157 = AXIS2_PLACEMENT_3D ( 'NONE', #5534, #4282, #669 ) ;
#10158 = ORIENTED_EDGE ( 'NONE', *, *, #339, .T. ) ;
#10159 = CARTESIAN_POINT ( 'NONE',  ( 27.86173033120691045, -69.39711819508849544, 3.710481764567783891 ) ) ;
#10160 = CARTESIAN_POINT ( 'NONE',  ( 8.850040237151072020, -60.00774340954457386, -2.531751357931705915 ) ) ;
#10161 = CARTESIAN_POINT ( 'NONE',  ( -24.54301448188264700, 2.673459138797629198, -47.50000001881890910 ) ) ;
#10162 = CARTESIAN_POINT ( 'NONE',  ( 8.902686789877913398, -55.58469383501344652, -2.908670588548444513 ) ) ;
#10163 = VERTEX_POINT ( 'NONE', #873 ) ;
#10164 = FACE_OUTER_BOUND ( 'NONE', #4137, .T. ) ;
#10165 = CARTESIAN_POINT ( 'NONE',  ( 69.97972559857382180, -3.172990593254279457, 75.19766410831374515 ) ) ;
#10166 = CARTESIAN_POINT ( 'NONE',  ( -24.96222495693456978, -7.431276100536581275, 57.50000000000012079 ) ) ;
#10167 = ADVANCED_FACE ( 'NONE', ( #4498 ), #13733, .T. ) ;
#10168 = CARTESIAN_POINT ( 'NONE',  ( -9.456839514482961562, 2.659958822950721391, 48.37147253714708484 ) ) ;
#10169 = CARTESIAN_POINT ( 'NONE',  ( 13.92771027672946538, -66.12098470289652141, -4.407543342774863149 ) ) ;
#10170 = VECTOR ( 'NONE', #11428, 1000.000000000000000 ) ;
#10171 = ADVANCED_FACE ( 'NONE', ( #14880 ), #4332, .F. ) ;
#10172 = ORIENTED_EDGE ( 'NONE', *, *, #10928, .F. ) ;
#10173 = ADVANCED_FACE ( 'NONE', ( #7887 ), #6647, .T. ) ;
#10174 = FACE_OUTER_BOUND ( 'NONE', #10525, .T. ) ;
#10175 = CARTESIAN_POINT ( 'NONE',  ( 50.01091543003727224, 23.25070940071368852, 139.1143251403882459 ) ) ;
#10176 = ORIENTED_EDGE ( 'NONE', *, *, #11631, .F. ) ;
#10177 =( LENGTH_UNIT ( ) NAMED_UNIT ( * ) SI_UNIT ( .MILLI., .METRE. ) );
#10178 = DIRECTION ( 'NONE',  ( 0.5006040828730989878, -0.8656763553492631269, 0.000000000000000000 ) ) ;
#10179 = EDGE_CURVE ( 'NONE', #1863, #2944, #2032, .T. ) ;
#10180 = DIRECTION ( 'NONE',  ( 1.000000000000000000, 0.000000000000000000, 0.000000000000000000 ) ) ;
#10181 = DIRECTION ( 'NONE',  ( -0.000000000000000000, 0.000000000000000000, -1.000000000000000000 ) ) ;
#10182 = ORIENTED_EDGE ( 'NONE', *, *, #12197, .F. ) ;
#10183 = DIRECTION ( 'NONE',  ( -0.000000000000000000, -0.000000000000000000, -1.000000000000000000 ) ) ;
#10184 = CARTESIAN_POINT ( 'NONE',  ( 9.665516716332046343, -61.13769932686095387, 2.043477119560002997 ) ) ;
#10185 = CARTESIAN_POINT ( 'NONE',  ( 20.86173033120691045, -52.24929059928630437, 0.000000000000000000 ) ) ;
#10186 = CARTESIAN_POINT ( 'NONE',  ( -12.99999999999998757, -67.96969602390581144, -32.99999999999998579 ) ) ;
#10187 = CARTESIAN_POINT ( 'NONE',  ( -24.96151347116557062, -6.448033549061094938, -47.50000000626571506 ) ) ;
#10188 = ORIENTED_EDGE ( 'NONE', *, *, #8257, .T. ) ;
#10189 = ORIENTED_EDGE ( 'NONE', *, *, #11036, .T. ) ;
#10190 = CARTESIAN_POINT ( 'NONE',  ( 24.18480965114325443, -70.79589105110501634, -6.161139702144090791 ) ) ;
#10191 = EDGE_CURVE ( 'NONE', #14840, #1587, #2106, .T. ) ;
#10192 = ORIENTED_EDGE ( 'NONE', *, *, #974, .F. ) ;
#10193 = PLANE ( 'NONE',  #2991 ) ;
#10194 = DIRECTION ( 'NONE',  ( 0.000000000000000000, 0.000000000000000000, 1.000000000000000000 ) ) ;
#10195 = VERTEX_POINT ( 'NONE', #1105 ) ;
#10196 = LINE ( 'NONE', #12420, #9905 ) ;
#10197 = LINE ( 'NONE', #4414, #6791 ) ;
#10198 = CARTESIAN_POINT ( 'NONE',  ( 9.234879212749161681, -60.63355790302721715, -1.939046661991500775 ) ) ;
#10199 = DIRECTION ( 'NONE',  ( 1.000000000000000000, 3.565820478396769525E-15, 0.000000000000000000 ) ) ;
#10200 = CARTESIAN_POINT ( 'NONE',  ( 33.04962008503242998, -54.34759098445695713, -2.119831996268577434 ) ) ;
#10201 = LINE ( 'NONE', #6732, #3948 ) ;
#10202 = CARTESIAN_POINT ( 'NONE',  ( 62.14609464170151654, 0.6526447315840442354, 60.61639468829817190 ) ) ;
#10203 = CARTESIAN_POINT ( 'NONE',  ( 67.21328690825529861, 29.52935533987996664, 21.00807340887166674 ) ) ;
#10204 = VERTEX_POINT ( 'NONE', #6726 ) ;
#10205 = CARTESIAN_POINT ( 'NONE',  ( 13.73837678375945792, -66.12497772680900709, -4.110792498370603454 ) ) ;
#10206 = EDGE_CURVE ( 'NONE', #13687, #7654, #8040, .T. ) ;
#10207 = EDGE_CURVE ( 'NONE', #13012, #8509, #11410, .T. ) ;
#10208 = ORIENTED_EDGE ( 'NONE', *, *, #667, .F. ) ;
#10209 = CARTESIAN_POINT ( 'NONE',  ( 31.30135442942146540, -53.71252461569495296, -3.555803702006928635 ) ) ;
#10210 = EDGE_LOOP ( 'NONE', ( #10615, #2932, #5011, #7594 ) ) ;
#10211 = CARTESIAN_POINT ( 'NONE',  ( 27.86188286885952081, -69.45278782524461292, 3.616934341765145167 ) ) ;
#10212 = DIRECTION ( 'NONE',  ( 0.000000000000000000, -1.000000000000000000, 0.000000000000000000 ) ) ;
#10213 = CARTESIAN_POINT ( 'NONE',  ( -16.99999999999998579, -2.249290599286303927, 47.50000000000012079 ) ) ;
#10214 = LINE ( 'NONE', #3131, #3539 ) ;
#10215 = DIRECTION ( 'NONE',  ( 0.000000000000000000, -1.000000000000000000, 0.000000000000000000 ) ) ;
#10216 = EDGE_LOOP ( 'NONE', ( #8117, #1559, #10828, #14134, #1445, #11530, #13797, #3364, #2685, #5002, #3221, #6478, #7184 ) ) ;
#10217 = CARTESIAN_POINT ( 'NONE',  ( -25.21252699837112132, -6.998437922861946880, 58.00000000000012079 ) ) ;
#10218 = CARTESIAN_POINT ( 'NONE',  ( 9.844272519834872170, -54.14181112192125767, -3.331498666157651112 ) ) ;
#10219 = FACE_OUTER_BOUND ( 'NONE', #13117, .T. ) ;
#10220 = DIRECTION ( 'NONE',  ( -0.8746197071345558349, 0.4848096202550685185, 0.000000000000000000 ) ) ;
#10221 = ORIENTED_EDGE ( 'NONE', *, *, #12225, .F. ) ;
#10222 = VERTEX_POINT ( 'NONE', #10348 ) ;
#10223 = EDGE_CURVE ( 'NONE', #3495, #14121, #14662, .T. ) ;
#10224 = CIRCLE ( 'NONE', #13401, 1.000000000000000888 ) ;
#10225 = EDGE_CURVE ( 'NONE', #8448, #5660, #5748, .T. ) ;
#10226 = ORIENTED_EDGE ( 'NONE', *, *, #2123, .F. ) ;
#10227 = CYLINDRICAL_SURFACE ( 'NONE', #6684, 4.194885682588113340 ) ;
#10228 = ORIENTED_EDGE ( 'NONE', *, *, #11701, .F. ) ;
#10229 = ORIENTED_EDGE ( 'NONE', *, *, #7029, .F. ) ;
#10230 = CARTESIAN_POINT ( 'NONE',  ( 68.90181265608016759, -8.292264031936127822, 71.19766410831374515 ) ) ;
#10231 = CARTESIAN_POINT ( 'NONE',  ( -23.91311688008704905, 3.524160940036151324, -47.66502101098827637 ) ) ;
#10232 = CIRCLE ( 'NONE', #6542, 0.7892041907098262810 ) ;
#10233 = CARTESIAN_POINT ( 'NONE',  ( 9.658440193288580389, -54.31466325532910844, -3.256939328598943195 ) ) ;
#10234 = CIRCLE ( 'NONE', #2614, 3.999999999999999112 ) ;
#10235 = DIRECTION ( 'NONE',  ( -0.000000000000000000, -0.000000000000000000, -1.000000000000000000 ) ) ;
#10236 = VERTEX_POINT ( 'NONE', #10432 ) ;
#10237 = CARTESIAN_POINT ( 'NONE',  ( 64.61411691182244965, -11.63232581036083069, 73.19766410831374515 ) ) ;
#10238 = CARTESIAN_POINT ( 'NONE',  ( 69.43429300475483501, -3.089800330891553148, 76.78179314627131191 ) ) ;
#10239 = CARTESIAN_POINT ( 'NONE',  ( -7.999999999999986677, -2.249290599286302594, 58.00000000000012079 ) ) ;
#10240 = FACE_OUTER_BOUND ( 'NONE', #10409, .T. ) ;
#10241 = CIRCLE ( 'NONE', #12455, 7.000000000000000000 ) ;
#10242 = EDGE_LOOP ( 'NONE', ( #10469, #7028, #9967, #1674 ) ) ;
#10243 = CARTESIAN_POINT ( 'NONE',  ( -5.040221427466046400, 4.089237592873870675, 48.50000000000012079 ) ) ;
#10244 = CIRCLE ( 'NONE', #12960, 1.000000000000000888 ) ;
#10245 = AXIS2_PLACEMENT_3D ( 'NONE', #4755, #213, #7209 ) ;
#10246 = LINE ( 'NONE', #14939, #7385 ) ;
#10247 = EDGE_CURVE ( 'NONE', #72, #4346, #13430, .T. ) ;
#10248 = ORIENTED_EDGE ( 'NONE', *, *, #14140, .F. ) ;
#10249 = CARTESIAN_POINT ( 'NONE',  ( 65.00000000000001421, -87.24929059928631148, 19.99999999999999645 ) ) ;
#10250 = LINE ( 'NONE', #12404, #11045 ) ;
#10251 = VERTEX_POINT ( 'NONE', #9042 ) ;
#10252 =( NAMED_UNIT ( * ) SI_UNIT ( $, .STERADIAN. ) SOLID_ANGLE_UNIT ( ) );
#10253 = LINE ( 'NONE', #1932, #15186 ) ;
#10254 = DIRECTION ( 'NONE',  ( 0.000000000000000000, 0.000000000000000000, -1.000000000000000000 ) ) ;
#10255 = ORIENTED_EDGE ( 'NONE', *, *, #11943, .T. ) ;
#10256 = VECTOR ( 'NONE', #1352, 1000.000000000000000 ) ;
#10257 = CARTESIAN_POINT ( 'NONE',  ( -8.787473001628836045, 2.499856724289236887, -48.50000000000012079 ) ) ;
#10258 = AXIS2_PLACEMENT_3D ( 'NONE', #6886, #7891, #10199 ) ;
#10259 = AXIS2_PLACEMENT_3D ( 'NONE', #5175, #4083, #9881 ) ;
#10260 = FACE_OUTER_BOUND ( 'NONE', #13413, .T. ) ;
#10261 = CARTESIAN_POINT ( 'NONE',  ( 30.86550480701848542, -53.50274931745886420, 3.718097397461435083 ) ) ;
#10262 = CARTESIAN_POINT ( 'NONE',  ( 20.86173033120691045, -82.24929059928629727, 0.000000000000000000 ) ) ;
#10263 = ADVANCED_FACE ( 'NONE', ( #4574 ), #4652, .T. ) ;
#10264 = DIRECTION ( 'NONE',  ( 0.000000000000000000, 0.000000000000000000, 1.000000000000000000 ) ) ;
#10265 = VERTEX_POINT ( 'NONE', #13969 ) ;
#10266 = AXIS2_PLACEMENT_3D ( 'NONE', #12925, #11828, #7067 ) ;
#10267 = ORIENTED_EDGE ( 'NONE', *, *, #7083, .T. ) ;
#10268 = DIRECTION ( 'NONE',  ( -2.312964634635742895E-17, -1.000000000000000000, 0.000000000000000000 ) ) ;
#10269 = VECTOR ( 'NONE', #3047, 1000.000000000000000 ) ;
#10270 = ORIENTED_EDGE ( 'NONE', *, *, #7384, .T. ) ;
#10271 = CARTESIAN_POINT ( 'NONE',  ( -16.99999999999998579, -2.249290599286303927, 36.00000000000012079 ) ) ;
#10272 = LINE ( 'NONE', #6878, #1764 ) ;
#10273 = VECTOR ( 'NONE', #2566, 1000.000000000000000 ) ;
#10274 = AXIS2_PLACEMENT_3D ( 'NONE', #4065, #13387, #12096 ) ;
#10275 = ORIENTED_EDGE ( 'NONE', *, *, #14302, .T. ) ;
#10276 = CARTESIAN_POINT ( 'NONE',  ( -30.80945343098651890, -5.389243620311580329, 48.00000000000012079 ) ) ;
#10277 = CARTESIAN_POINT ( 'NONE',  ( 80.00000000000001421, -74.24929059928631148, -4.000000000000000000 ) ) ;
#10278 = ADVANCED_FACE ( 'NONE', ( #3341 ), #12744, .F. ) ;
#10279 = EDGE_CURVE ( 'NONE', #11241, #13684, #6881, .T. ) ;
#10280 = CARTESIAN_POINT ( 'NONE',  ( 9.369121201332232474, -60.80954383512729322, -1.970170733381408024 ) ) ;
#10281 = VECTOR ( 'NONE', #7314, 1000.000000000000000 ) ;
#10282 = CARTESIAN_POINT ( 'NONE',  ( 57.92627403409715470, 23.25070940071368852, 84.20452624982236500 ) ) ;
#10283 = CARTESIAN_POINT ( 'NONE',  ( 31.95734593916283472, -60.25982778069333534, 2.890715052751938074 ) ) ;
#10284 = FACE_OUTER_BOUND ( 'NONE', #5421, .T. ) ;
#10285 = CIRCLE ( 'NONE', #14221, 0.7892041907098262810 ) ;
#10286 = DIRECTION ( 'NONE',  ( -1.000000000000000000, -8.673617379884035472E-17, 0.000000000000000000 ) ) ;
#10287 = LINE ( 'NONE', #3278, #7801 ) ;
#10288 = ORIENTED_EDGE ( 'NONE', *, *, #11053, .F. ) ;
#10289 = CARTESIAN_POINT ( 'NONE',  ( 13.13093853397579380, -57.14744317414096031, -4.208698379210318308 ) ) ;
#10290 = EDGE_LOOP ( 'NONE', ( #11747, #13243, #4289, #9098, #15162 ) ) ;
#10291 = CARTESIAN_POINT ( 'NONE',  ( 109.8334623555409735, 23.25070940071369563, -33.00000000000012790 ) ) ;
#10292 = VERTEX_POINT ( 'NONE', #8119 ) ;
#10293 = CARTESIAN_POINT ( 'NONE',  ( 12.47090034640682354, -63.08803683229641024, -3.873126822354290955 ) ) ;
#10294 = LINE ( 'NONE', #13986, #14179 ) ;
#10295 = DIRECTION ( 'NONE',  ( -1.000000000000000000, -0.000000000000000000, -0.000000000000000000 ) ) ;
#10296 = CYLINDRICAL_SURFACE ( 'NONE', #1573, 4.000000000000000000 ) ;
#10297 = CARTESIAN_POINT ( 'NONE',  ( -12.09280073291247426, -85.24929059928631148, -11.78977872328358067 ) ) ;
#10298 = ORIENTED_EDGE ( 'NONE', *, *, #6946, .T. ) ;
#10299 = ADVANCED_FACE ( 'NONE', ( #12819 ), #3503, .F. ) ;
#10300 = CARTESIAN_POINT ( 'NONE',  ( 66.38598137497019991, -11.47113225237460910, 76.19766410831374515 ) ) ;
#10301 = CARTESIAN_POINT ( 'NONE',  ( 8.821484763567296383, -57.33450387999030795, -2.749014434309872801 ) ) ;
#10302 = CARTESIAN_POINT ( 'NONE',  ( -16.99999999999998579, -2.249290599286303927, 57.50000000000012079 ) ) ;
#10303 = CARTESIAN_POINT ( 'NONE',  ( -12.14523415828302078, -9.827631355817260328, 48.50000000000012079 ) ) ;
#10304 = ORIENTED_EDGE ( 'NONE', *, *, #7447, .T. ) ;
#10305 = DIRECTION ( 'NONE',  ( 1.000000000000000000, 0.000000000000000000, 0.000000000000000000 ) ) ;
#10306 = ORIENTED_EDGE ( 'NONE', *, *, #11719, .T. ) ;
#10307 = LINE ( 'NONE', #13918, #2766 ) ;
#10308 = ORIENTED_EDGE ( 'NONE', *, *, #10722, .T. ) ;
#10309 = DIRECTION ( 'NONE',  ( 0.000000000000000000, 0.000000000000000000, -1.000000000000000000 ) ) ;
#10310 = CARTESIAN_POINT ( 'NONE',  ( -21.85476584171706449, 5.329050157244580532, -48.50000000000012079 ) ) ;
#10311 = VECTOR ( 'NONE', #12729, 1000.000000000000000 ) ;
#10312 = FACE_BOUND ( 'NONE', #820, .T. ) ;
#10313 = EDGE_CURVE ( 'NONE', #10836, #4409, #183, .T. ) ;
#10314 = ADVANCED_FACE ( 'NONE', ( #14356 ), #13122, .T. ) ;
#10315 = ORIENTED_EDGE ( 'NONE', *, *, #1043, .T. ) ;
#10316 = PRODUCT_DEFINITION ( 'UNKNOWN', '', #5588, #12123 ) ;
#10317 = CARTESIAN_POINT ( 'NONE',  ( 25.81270058232203013, 23.25070940071368852, 33.00000000000012790 ) ) ;
#10318 = DIRECTION ( 'NONE',  ( 0.000000000000000000, 0.000000000000000000, 1.000000000000000000 ) ) ;
#10319 = DIRECTION ( 'NONE',  ( 0.8656763553492639041, 0.5006040828730973224, -0.000000000000000000 ) ) ;
#10320 = CARTESIAN_POINT ( 'NONE',  ( 16.19116130666622766, -53.25924492462442572, -5.664691252382128894 ) ) ;
#10321 = CARTESIAN_POINT ( 'NONE',  ( 34.39304362052245523, -50.37435811137176955, 2.733270616923093588 ) ) ;
#10322 = EDGE_LOOP ( 'NONE', ( #1315, #6367, #5144, #527 ) ) ;
#10323 = CARTESIAN_POINT ( 'NONE',  ( 69.43190845037254633, -3.121612608933937327, 71.58974242810022304 ) ) ;
#10324 = CIRCLE ( 'NONE', #6387, 11.46463184759104692 ) ;
#10325 = DIRECTION ( 'NONE',  ( 0.000000000000000000, 0.000000000000000000, -1.000000000000000000 ) ) ;
#10326 = ORIENTED_EDGE ( 'NONE', *, *, #7259, .T. ) ;
#10327 = DIRECTION ( 'NONE',  ( 0.000000000000000000, 0.000000000000000000, -1.000000000000000000 ) ) ;
#10328 = LINE ( 'NONE', #13786, #3426 ) ;
#10329 =( NAMED_UNIT ( * ) PLANE_ANGLE_UNIT ( ) SI_UNIT ( $, .RADIAN. ) );
#10330 = CARTESIAN_POINT ( 'NONE',  ( -9.271822474830681671, -6.861803161813159413, -48.00000000000019895 ) ) ;
#10331 = DIRECTION ( 'NONE',  ( -1.000000000000000000, 0.000000000000000000, 0.000000000000000000 ) ) ;
#10332 = EDGE_LOOP ( 'NONE', ( #7926, #14712, #12796, #3951 ) ) ;
#10333 = EDGE_CURVE ( 'NONE', #5415, #10867, #6202, .T. ) ;
#10334 = FACE_OUTER_BOUND ( 'NONE', #2958, .T. ) ;
#10335 = AXIS2_PLACEMENT_3D ( 'NONE', #11091, #4010, #7488 ) ;
#10336 = DIRECTION ( 'NONE',  ( 1.000000000000000000, 0.000000000000000000, 0.000000000000000000 ) ) ;
#10337 = CARTESIAN_POINT ( 'NONE',  ( 32.06502046912525827, -54.31466325532912975, 3.256939328598943639 ) ) ;
#10338 = CARTESIAN_POINT ( 'NONE',  ( 9.074525391310594102, -58.48797006926987763, 2.754379914540423524 ) ) ;
#10339 = DIRECTION ( 'NONE',  ( 0.7915791710638007128, 0.6110666215217015473, 0.000000000000000000 ) ) ;
#10340 = EDGE_LOOP ( 'NONE', ( #6083, #2857, #1103, #13445 ) ) ;
#10341 = CIRCLE ( 'NONE', #13530, 9.000000000000001776 ) ;
#10342 = CARTESIAN_POINT ( 'NONE',  ( 27.98566521725750178, -66.12426320361456078, -4.110478850071108248 ) ) ;
#10343 = ORIENTED_EDGE ( 'NONE', *, *, #10547, .F. ) ;
#10344 = CARTESIAN_POINT ( 'NONE',  ( 27.60269520869858439, -53.27034158699310495, -4.884662653952261735 ) ) ;
#10345 = DIRECTION ( 'NONE',  ( -1.000000000000000000, 0.000000000000000000, 0.000000000000000000 ) ) ;
#10346 = VERTEX_POINT ( 'NONE', #10889 ) ;
#10347 = DIRECTION ( 'NONE',  ( -0.000000000000000000, 1.000000000000000000, 1.445602896647339163E-16 ) ) ;
#10348 = CARTESIAN_POINT ( 'NONE',  ( 31.72322230991231962, -61.42570632716525125, -2.132522520905369312 ) ) ;
#10349 = EDGE_CURVE ( 'NONE', #14228, #7395, #346, .T. ) ;
#10350 = TOROIDAL_SURFACE ( 'NONE', #12310, 4.165819364273509962, 0.5000000000000000000 ) ;
#10351 = PRESENTATION_STYLE_ASSIGNMENT (( #8121 ) ) ;
#10352 = VECTOR ( 'NONE', #14093, 1000.000000000000000 ) ;
#10353 = FACE_OUTER_BOUND ( 'NONE', #4830, .T. ) ;
#10354 = DIRECTION ( 'NONE',  ( 1.000000000000000000, 0.000000000000000000, 0.000000000000000000 ) ) ;
#10355 = DIRECTION ( 'NONE',  ( -1.000000000000000000, -0.000000000000000000, -0.000000000000000000 ) ) ;
#10356 = DIRECTION ( 'NONE',  ( 0.000000000000000000, -0.000000000000000000, -1.000000000000000000 ) ) ;
#10357 = LINE ( 'NONE', #12510, #12733 ) ;
#10358 = EDGE_CURVE ( 'NONE', #9144, #13981, #8432, .T. ) ;
#10359 = ORIENTED_EDGE ( 'NONE', *, *, #707, .F. ) ;
#10360 = EDGE_CURVE ( 'NONE', #7307, #7221, #13694, .T. ) ;
#10361 = CARTESIAN_POINT ( 'NONE',  ( 17.93383279432269006, -62.59345883550169987, -6.358786672823088182 ) ) ;
#10362 = AXIS2_PLACEMENT_3D ( 'NONE', #12988, #2436, #11815 ) ;
#10363 = AXIS2_PLACEMENT_3D ( 'NONE', #12866, #3766, #2384 ) ;
#10364 = ORIENTED_EDGE ( 'NONE', *, *, #8857, .T. ) ;
#10365 = CARTESIAN_POINT ( 'NONE',  ( 32.77533487224304309, -57.91121052158847249, -2.751677492798594749 ) ) ;
#10366 = VECTOR ( 'NONE', #13344, 1000.000000000000000 ) ;
#10367 = ORIENTED_EDGE ( 'NONE', *, *, #9837, .T. ) ;
#10368 = LINE ( 'NONE', #9140, #11062 ) ;
#10369 = CARTESIAN_POINT ( 'NONE',  ( -5.040221427466112125, 4.089237592873837812, 57.50000000000012079 ) ) ;
#10370 = ADVANCED_FACE ( 'NONE', ( #4887 ), #7064, .F. ) ;
#10371 = DIRECTION ( 'NONE',  ( -0.000000000000000000, 0.000000000000000000, -1.000000000000000000 ) ) ;
#10372 = DIRECTION ( 'NONE',  ( 0.000000000000000000, 1.000000000000000000, 1.734723475976805517E-15 ) ) ;
#10373 = ORIENTED_EDGE ( 'NONE', *, *, #7912, .F. ) ;
#10374 = AXIS2_PLACEMENT_3D ( 'NONE', #7035, #12970, #4648 ) ;
#10375 = AXIS2_PLACEMENT_3D ( 'NONE', #9396, #14393, #1459 ) ;
#10376 = CARTESIAN_POINT ( 'NONE',  ( 65.14440678340884006, -11.91619605160587803, 75.34954452637725808 ) ) ;
#10377 = CARTESIAN_POINT ( 'NONE',  ( 9.585944920971037675, -54.40403913628145460, -3.226152465599050778 ) ) ;
#10378 = CARTESIAN_POINT ( 'NONE',  ( 24.62796245282055452, -96.56299909827106376, 1.347403282660977419 ) ) ;
#10379 = CARTESIAN_POINT ( 'NONE',  ( -12.14523415828302078, -9.827631355817260328, 48.50000000000012079 ) ) ;
#10380 = EDGE_LOOP ( 'NONE', ( #7149, #6038, #11924, #3980 ) ) ;
#10381 = ORIENTED_EDGE ( 'NONE', *, *, #14052, .T. ) ;
#10382 = CYLINDRICAL_SURFACE ( 'NONE', #12213, 7.000000000000000000 ) ;
#10383 = VERTEX_POINT ( 'NONE', #13045 ) ;
#10384 = DIRECTION ( 'NONE',  ( -0.8420378618367727608, -0.5394184268574406804, -0.000000000000000000 ) ) ;
#10385 = ORIENTED_EDGE ( 'NONE', *, *, #1335, .T. ) ;
#10386 = CIRCLE ( 'NONE', #10629, 8.924024642120691908 ) ;
#10387 = VECTOR ( 'NONE', #13151, 1000.000000000000000 ) ;
#10388 = EDGE_CURVE ( 'NONE', #13060, #3246, #14920, .T. ) ;
#10389 = ORIENTED_EDGE ( 'NONE', *, *, #12736, .F. ) ;
#10390 = VECTOR ( 'NONE', #1398, 1000.000000000000000 ) ;
#10391 = DIRECTION ( 'NONE',  ( -0.000000000000000000, -0.000000000000000000, 1.000000000000000000 ) ) ;
#10392 = CARTESIAN_POINT ( 'NONE',  ( -24.57377864815406099, 2.621914368698142983, -47.92899112040971943 ) ) ;
#10393 = CIRCLE ( 'NONE', #4235, 9.999999999999994671 ) ;
#10394 = CARTESIAN_POINT ( 'NONE',  ( -12.14523415828296216, -9.827631355817223024, 48.50000000000012079 ) ) ;
#10395 = CARTESIAN_POINT ( 'NONE',  ( 84.72310019870096198, 25.52935533987996664, -33.00000000000013500 ) ) ;
#10396 = EDGE_LOOP ( 'NONE', ( #3604, #2257, #939, #12129, #13492, #2726, #7987 ) ) ;
#10397 = CYLINDRICAL_SURFACE ( 'NONE', #3656, 2.499999999999995115 ) ;
#10398 = VECTOR ( 'NONE', #9432, 1000.000000000000000 ) ;
#10399 = CARTESIAN_POINT ( 'NONE',  ( 32.94091731014317048, -56.07132046089822097, -2.830553478268885481 ) ) ;
#10400 = CARTESIAN_POINT ( 'NONE',  ( 29.70251902843243030, -52.24929059928630437, 4.175384597093452221 ) ) ;
#10401 = CARTESIAN_POINT ( 'NONE',  ( 28.78836361348337647, -54.57042255627918337, 4.214900875688467607 ) ) ;
#10402 = ORIENTED_EDGE ( 'NONE', *, *, #11023, .T. ) ;
#10403 = AXIS2_PLACEMENT_3D ( 'NONE', #9377, #14072, #4761 ) ;
#10404 = CARTESIAN_POINT ( 'NONE',  ( 69.30279253104961867, -4.172890756685618818, 72.15742259932318348 ) ) ;
#10405 = AXIS2_PLACEMENT_3D ( 'NONE', #13092, #14169, #8330 ) ;
#10406 = CARTESIAN_POINT ( 'NONE',  ( 16.55198862119814862, -52.24929059928630437, 4.731953141213115721 ) ) ;
#10407 = EDGE_CURVE ( 'NONE', #4043, #13455, #1406, .T. ) ;
#10408 = B_SPLINE_CURVE_WITH_KNOTS ( 'NONE', 3,
 ( #6077, #1451, #12147, #6159 ),
 .UNSPECIFIED., .F., .F.,
 ( 4, 4 ),
 ( 0.000000000000000000, 0.006642668954637880041 ),
 .UNSPECIFIED. ) ;
#10409 = EDGE_LOOP ( 'NONE', ( #13917, #1550, #11772, #9963 ) ) ;
#10410 = EDGE_CURVE ( 'NONE', #13060, #7307, #11729, .T. ) ;
#10411 = SHAPE_REPRESENTATION ( 'L-Shaped Aluminum Bracket', ( #6315 ), #4594 ) ;
#10412 = FILL_AREA_STYLE_COLOUR ( '', #4405 ) ;
#10413 = DIRECTION ( 'NONE',  ( 0.000000000000000000, 0.000000000000000000, 1.000000000000000000 ) ) ;
#10414 = LINE ( 'NONE', #7948, #923 ) ;
#10415 = LINE ( 'NONE', #3092, #1041 ) ;
#10416 = ORIENTED_EDGE ( 'NONE', *, *, #4923, .F. ) ;
#10417 = CARTESIAN_POINT ( 'NONE',  ( 0.000000000000000000, 21.75070940071366365, 13.14990448602693007 ) ) ;
#10418 = VECTOR ( 'NONE', #1956, 1000.000000000000000 ) ;
#10419 = CARTESIAN_POINT ( 'NONE',  ( 75.52271037289314393, -7.388871293676331220, 73.19766410831374515 ) ) ;
#10420 = EDGE_CURVE ( 'NONE', #3522, #8564, #2640, .T. ) ;
#10421 = DIRECTION ( 'NONE',  ( 0.000000000000000000, -0.000000000000000000, -1.000000000000000000 ) ) ;
#10422 = CARTESIAN_POINT ( 'NONE',  ( -5.040221427466109461, 4.089237592873834259, 48.00000000000012079 ) ) ;
#10423 = LINE ( 'NONE', #4563, #10311 ) ;
#10424 = ORIENTED_EDGE ( 'NONE', *, *, #12393, .T. ) ;
#10425 = EDGE_CURVE ( 'NONE', #14061, #6293, #9023, .T. ) ;
#10426 = CARTESIAN_POINT ( 'NONE',  ( 31.77372435728965883, -63.13800426661170206, -2.713090553711066555 ) ) ;
#10427 = EDGE_LOOP ( 'NONE', ( #4448, #6281, #4884, #5571 ) ) ;
#10428 = CARTESIAN_POINT ( 'NONE',  ( 11.00828597368551698, -52.46167102156725548, -2.825639067667213844 ) ) ;
#10429 = LINE ( 'NONE', #12578, #11856 ) ;
#10430 = ORIENTED_EDGE ( 'NONE', *, *, #5485, .F. ) ;
#10431 = CARTESIAN_POINT ( 'NONE',  ( 65.00000000000001421, -85.27429059928628874, -19.99999999999999645 ) ) ;
#10432 = CARTESIAN_POINT ( 'NONE',  ( -24.72817752516938228, 2.363221963240404566, 47.50000000000012079 ) ) ;
#10433 = CARTESIAN_POINT ( 'NONE',  ( -65.00000000000001421, -85.24929059928629727, -19.99999999999999645 ) ) ;
#10434 = CARTESIAN_POINT ( 'NONE',  ( -12.83418063572647760, -2.249290599286303927, 50.00000000000012079 ) ) ;
#10435 = CARTESIAN_POINT ( 'NONE',  ( -2.016677571526633510E-15, 23.25070940071368497, 33.00000000000012790 ) ) ;
#10436 = DIRECTION ( 'NONE',  ( -0.000000000000000000, -0.000000000000000000, 1.000000000000000000 ) ) ;
#10437 = CARTESIAN_POINT ( 'NONE',  ( 17.61519226005271577, -69.39711819508866597, -6.201611931792120558 ) ) ;
#10438 = ORIENTED_EDGE ( 'NONE', *, *, #6532, .F. ) ;
#10439 = DIRECTION ( 'NONE',  ( -1.000000000000000000, 9.251858538542971581E-17, -0.000000000000000000 ) ) ;
#10440 = PRODUCT_DEFINITION_CONTEXT ( 'detailed design', #14881, 'design' ) ;
#10441 = ORIENTED_EDGE ( 'NONE', *, *, #740, .T. ) ;
#10442 = DIRECTION ( 'NONE',  ( 0.000000000000000000, 1.000000000000000000, -0.000000000000000000 ) ) ;
#10443 = ORIENTED_EDGE ( 'NONE', *, *, #2601, .F. ) ;
#10444 = CARTESIAN_POINT ( 'NONE',  ( 14.39660743346648708, -68.54652648479442689, -4.542640093672132728 ) ) ;
#10445 = SURFACE_STYLE_USAGE ( .BOTH. , #4143 ) ;
#10446 = EDGE_CURVE ( 'NONE', #13020, #7467, #41, .T. ) ;
#10447 = DIRECTION ( 'NONE',  ( 8.673617379884035472E-17, -1.000000000000000000, 0.000000000000000000 ) ) ;
#10448 = CARTESIAN_POINT ( 'NONE',  ( 108.0866310645538562, 23.25070940071369563, -13.14990448602692474 ) ) ;
#10449 = EDGE_CURVE ( 'NONE', #2182, #5691, #3368, .T. ) ;
#10450 = EDGE_CURVE ( 'NONE', #3036, #14454, #12028, .T. ) ;
#10451 = ORIENTED_EDGE ( 'NONE', *, *, #6045, .T. ) ;
#10452 = DIRECTION ( 'NONE',  ( 0.000000000000000000, 0.000000000000000000, -1.000000000000000000 ) ) ;
#10453 = CARTESIAN_POINT ( 'NONE',  ( 8.152528251094548040, -55.78447712832181082, -2.622266312281611000 ) ) ;
#10454 = CARTESIAN_POINT ( 'NONE',  ( 88.00000000000001421, 10.75070940071369208, 33.00000000000012790 ) ) ;
#10455 = CARTESIAN_POINT ( 'NONE',  ( -11.53791661996513085, -9.438577269332638409, 48.38299871084047510 ) ) ;
#10456 = EDGE_CURVE ( 'NONE', #302, #9144, #2397, .T. ) ;
#10457 = EDGE_LOOP ( 'NONE', ( #12897, #10443, #12003, #10766 ) ) ;
#10458 = CARTESIAN_POINT ( 'NONE',  ( 33.52235686305655804, -57.48563641131178770, 1.816685854991385574 ) ) ;
#10459 = ORIENTED_EDGE ( 'NONE', *, *, #10584, .F. ) ;
#10460 = DIRECTION ( 'NONE',  ( -0.000000000000000000, -1.000000000000000000, -0.000000000000000000 ) ) ;
#10461 = VERTEX_POINT ( 'NONE', #1414 ) ;
#10462 = ORIENTED_EDGE ( 'NONE', *, *, #196, .T. ) ;
#10463 = EDGE_CURVE ( 'NONE', #11541, #13742, #12973, .T. ) ;
#10464 = DIRECTION ( 'NONE',  ( 0.000000000000000000, -0.000000000000000000, 1.000000000000000000 ) ) ;
#10465 = DIRECTION ( 'NONE',  ( -0.9274945937977119303, 1.321628185579677547E-15, 0.3738365665314420383 ) ) ;
#10466 = EDGE_CURVE ( 'NONE', #10163, #13455, #1260, .T. ) ;
#10467 = CARTESIAN_POINT ( 'NONE',  ( 76.93272077111119245, -7.027098752189868236, 76.13615421477460643 ) ) ;
#10468 = LINE ( 'NONE', #15161, #15047 ) ;
#10469 = ORIENTED_EDGE ( 'NONE', *, *, #12810, .F. ) ;
#10470 = VECTOR ( 'NONE', #9944, 1000.000000000000114 ) ;
#10471 = LINE ( 'NONE', #4622, #12471 ) ;
#10472 = DIRECTION ( 'NONE',  ( 0.000000000000000000, 0.000000000000000000, 1.000000000000000000 ) ) ;
#10473 = ADVANCED_FACE ( 'NONE', ( #12256 ), #4015, .T. ) ;
#10474 = CARTESIAN_POINT ( 'NONE',  ( -16.99999999999998579, -2.249290599286305703, -115.4621125123531442 ) ) ;
#10475 = DIRECTION ( 'NONE',  ( -0.000000000000000000, -0.000000000000000000, -1.000000000000000000 ) ) ;
#10476 = EDGE_LOOP ( 'NONE', ( #5762, #13529, #6063, #5236 ) ) ;
#10477 = CARTESIAN_POINT ( 'NONE',  ( 70.12227446635188244, -3.653170910121650738, 72.43426084522523922 ) ) ;
#10478 = ORIENTED_EDGE ( 'NONE', *, *, #1656, .F. ) ;
#10479 = LINE ( 'NONE', #11780, #3501 ) ;
#10480 = DIRECTION ( 'NONE',  ( -0.9274945937977119303, -3.217893291404924306E-15, -0.3738365665314420383 ) ) ;
#10481 = AXIS2_PLACEMENT_3D ( 'NONE', #4937, #14253, #2322 ) ;
#10482 = CARTESIAN_POINT ( 'NONE',  ( -10.27534025206727186, -8.241935476752797030, -47.97348817130912835 ) ) ;
#10483 = DIRECTION ( 'NONE',  ( -0.8656763553492639041, -0.5006040828730973224, -0.000000000000000000 ) ) ;
#10484 = VERTEX_POINT ( 'NONE', #6404 ) ;
#10485 = EDGE_CURVE ( 'NONE', #11588, #4043, #11173, .T. ) ;
#10486 = FACE_OUTER_BOUND ( 'NONE', #8101, .T. ) ;
#10487 = CARTESIAN_POINT ( 'NONE',  ( 65.00000000000001421, -85.24929059928629727, -19.99999999999999645 ) ) ;
#10488 = EDGE_CURVE ( 'NONE', #8992, #1911, #6338, .T. ) ;
#10489 = LINE ( 'NONE', #14868, #676 ) ;
#10490 = DIRECTION ( 'NONE',  ( 0.000000000000000000, 1.000000000000000000, -0.000000000000000000 ) ) ;
#10491 = EDGE_CURVE ( 'NONE', #3380, #9847, #15172, .T. ) ;
#10492 = CARTESIAN_POINT ( 'NONE',  ( 18.00000000000001066, 15.25070940071368497, 33.00000000000012790 ) ) ;
#10493 = VECTOR ( 'NONE', #7302, 1000.000000000000000 ) ;
#10494 = DIRECTION ( 'NONE',  ( -0.000000000000000000, 0.000000000000000000, 1.000000000000000000 ) ) ;
#10495 = ORIENTED_EDGE ( 'NONE', *, *, #5807, .F. ) ;
#10496 =( BOUNDED_SURFACE ( )  B_SPLINE_SURFACE ( 3, 2, ( 
 ( #14968, #14731, #7662 ),
 ( #8806, #12355, #7584 ),
 ( #4182, #10122, #6427 ),
 ( #12277, #579, #1811 ),
 ( #8886, #6501, #10046 ),
 ( #8962, #13580, #11191 ),
 ( #3046, #11337, #7888 ),
 ( #7738, #14809, #12423 ),
 ( #1874, #13735, #12502 ),
 ( #2034, #3113, #1951 ),
 ( #798, #5513, #9043 ),
 ( #12585, #4575, #4737 ),
 ( #1193, #125, #2192 ),
 ( #12745, #10508, #3575 ) ),
 .UNSPECIFIED., .F., .F., .F. ) 
 B_SPLINE_SURFACE_WITH_KNOTS ( ( 4, 2, 2, 2, 2, 2, 4 ),
 ( 3, 3 ),
 ( 0.000000000000000000, 0.002560658414910375099, 0.003840987622365562432, 0.005121316829820750198, 0.006401646037275937964, 0.007681975244731124863, 0.01024263365964150040 ),
 ( 0.000000000000000000, 1.000000000000000000 ),
 .UNSPECIFIED. ) 
 GEOMETRIC_REPRESENTATION_ITEM ( )  RATIONAL_B_SPLINE_SURFACE ( (
 ( 1.000000000000000000, 0.8053615646146036200, 1.000000000000000000),
 ( 1.000000000000000000, 0.8105996499489666052, 1.000000000000000000),
 ( 1.000000000000000000, 0.8160199193855625088, 1.000000000000000000),
 ( 1.000000000000000000, 0.8240376314734160212, 1.000000000000000000),
 ( 1.000000000000000000, 0.8266971106455908158, 1.000000000000000000),
 ( 1.000000000000000000, 0.8319110421177055015, 1.000000000000000000),
 ( 1.000000000000000000, 0.8344214672177876491, 1.000000000000000000),
 ( 1.000000000000000000, 0.8392107060239100136, 1.000000000000000000),
 ( 1.000000000000000000, 0.8414897010531573462, 1.000000000000000000),
 ( 1.000000000000000000, 0.8457750297010532270, 1.000000000000000000),
 ( 1.000000000000000000, 0.8477871175334914522, 1.000000000000000000),
 ( 1.000000000000000000, 0.8533050377657773744, 1.000000000000000000),
 ( 1.000000000000000000, 0.8561733496718711978, 1.000000000000000000),
 ( 1.000000000000000000, 0.8581891718822912685, 1.000000000000000000) ) ) 
 REPRESENTATION_ITEM ( '' )  SURFACE ( )  );
#10497 = EDGE_LOOP ( 'NONE', ( #8155, #9196, #13575, #7095 ) ) ;
#10498 = CARTESIAN_POINT ( 'NONE',  ( 50.07597535787931520, -2.249290599286309256, 47.51982618741348574 ) ) ;
#10499 = CIRCLE ( 'NONE', #1152, 0.5000000000000004441 ) ;
#10500 = VERTEX_POINT ( 'NONE', #555 ) ;
#10501 = CARTESIAN_POINT ( 'NONE',  ( 8.098912479706312340, -56.24150114312890025, -1.860592018039514350 ) ) ;
#10502 = LINE ( 'NONE', #13189, #3504 ) ;
#10503 = CIRCLE ( 'NONE', #9271, 4.194885682588113340 ) ;
#10504 = ORIENTED_EDGE ( 'NONE', *, *, #174, .F. ) ;
#10505 = DIRECTION ( 'NONE',  ( -1.000000000000000000, -1.156482317317871725E-16, 0.000000000000000000 ) ) ;
#10506 = CARTESIAN_POINT ( 'NONE',  ( 54.03086304124234829, 0.8903401505190762233, 48.51982618741349285 ) ) ;
#10507 = VECTOR ( 'NONE', #9740, 1000.000000000000000 ) ;
#10508 = CARTESIAN_POINT ( 'NONE',  ( 13.86142555056148851, -69.48056866272027321, 4.214447830835809761 ) ) ;
#10509 = EDGE_CURVE ( 'NONE', #384, #1157, #3861, .T. ) ;
#10510 = ADVANCED_FACE ( 'NONE', ( #5260 ), #5843, .T. ) ;
#10511 = CYLINDRICAL_SURFACE ( 'NONE', #11975, 0.7892041907098261699 ) ;
#10512 = DIRECTION ( 'NONE',  ( -0.000000000000000000, -1.000000000000000000, -0.000000000000000000 ) ) ;
#10513 = CARTESIAN_POINT ( 'NONE',  ( -16.99999999999998579, 7.750709400713696517, 38.00000000000012079 ) ) ;
#10514 = AXIS2_PLACEMENT_3D ( 'NONE', #5592, #12666, #8051 ) ;
#10515 = CARTESIAN_POINT ( 'NONE',  ( 95.31453344691183815, 21.75070940071356418, -33.00000000000012790 ) ) ;
#10516 = VECTOR ( 'NONE', #4418, 1000.000000000000000 ) ;
#10517 = CARTESIAN_POINT ( 'NONE',  ( 31.49780332062879040, -53.83453582474924559, 3.481203917140397230 ) ) ;
#10518 = ORIENTED_EDGE ( 'NONE', *, *, #3436, .T. ) ;
#10519 = AXIS2_PLACEMENT_3D ( 'NONE', #6629, #1087, #2245 ) ;
#10520 = CARTESIAN_POINT ( 'NONE',  ( 18.13205847683729388, -57.03285117767155299, -6.445925775549026682 ) ) ;
#10521 = VERTEX_POINT ( 'NONE', #7561 ) ;
#10522 = CARTESIAN_POINT ( 'NONE',  ( -5.290523468902621929, 4.522075770548486418, 48.50000000000012079 ) ) ;
#10523 = ORIENTED_EDGE ( 'NONE', *, *, #6454, .T. ) ;
#10524 = CARTESIAN_POINT ( 'NONE',  ( -16.99999999999998579, -2.249290599286303927, 47.50000000000012079 ) ) ;
#10525 = EDGE_LOOP ( 'NONE', ( #6918, #6876, #6891, #1927 ) ) ;
#10526 = DIRECTION ( 'NONE',  ( -0.000000000000000000, -0.000000000000000000, -1.000000000000000000 ) ) ;
#10527 = DIRECTION ( 'NONE',  ( -0.000000000000000000, -0.000000000000000000, -1.000000000000000000 ) ) ;
#10528 = AXIS2_PLACEMENT_3D ( 'NONE', #3238, #96, #11778 ) ;
#10529 = CARTESIAN_POINT ( 'NONE',  ( 12.36791015745246369, -52.24929059928630437, -3.199931146564426232 ) ) ;
#10530 = AXIS2_PLACEMENT_3D ( 'NONE', #2914, #2483, #4795 ) ;
#10531 = EDGE_LOOP ( 'NONE', ( #9201, #10825, #7002, #11565, #7924, #8204, #9937, #5146, #12125, #2138, #11237 ) ) ;
#10532 = FACE_OUTER_BOUND ( 'NONE', #5, .T. ) ;
#10533 = DIRECTION ( 'NONE',  ( 0.000000000000000000, -0.000000000000000000, 1.000000000000000000 ) ) ;
#10534 = CARTESIAN_POINT ( 'NONE',  ( 72.26742264675378635, -14.73126838498886571, 75.19766410831374515 ) ) ;
#10535 = CARTESIAN_POINT ( 'NONE',  ( 20.86173033120691045, -72.24929059928631148, 0.000000000000000000 ) ) ;
#10536 = VERTEX_POINT ( 'NONE', #1572 ) ;
#10537 = ORIENTED_EDGE ( 'NONE', *, *, #503, .T. ) ;
#10538 = LINE ( 'NONE', #14911, #15166 ) ;
#10539 = ORIENTED_EDGE ( 'NONE', *, *, #4423, .T. ) ;
#10540 = CARTESIAN_POINT ( 'NONE',  ( 12.22370793440460801, -62.74348037527475697, 3.781439773221460854 ) ) ;
#10541 = EDGE_LOOP ( 'NONE', ( #353, #5848 ) ) ;
#10542 = ORIENTED_EDGE ( 'NONE', *, *, #4364, .F. ) ;
#10543 = EDGE_CURVE ( 'NONE', #14082, #9158, #3122, .T. ) ;
#10544 = DIRECTION ( 'NONE',  ( 1.156482317317870492E-16, -1.000000000000000000, 0.000000000000000000 ) ) ;
#10545 = DIRECTION ( 'NONE',  ( 0.000000000000000000, 0.000000000000000000, -1.000000000000000000 ) ) ;
#10546 = EDGE_CURVE ( 'NONE', #6843, #60, #8306, .T. ) ;
#10547 = EDGE_CURVE ( 'NONE', #12099, #12141, #4347, .T. ) ;
#10548 = LINE ( 'NONE', #11918, #9134 ) ;
#10549 = CARTESIAN_POINT ( 'NONE',  ( -8.537170960192302260, 2.067018546614596719, 48.00000000000012079 ) ) ;
#10550 = ORIENTED_EDGE ( 'NONE', *, *, #9510, .F. ) ;
#10551 = CARTESIAN_POINT ( 'NONE',  ( 58.00000000000000711, -2.249290599286311032, 33.00000000000012790 ) ) ;
#10552 = CARTESIAN_POINT ( 'NONE',  ( 109.8334623555409735, 0.000000000000000000, 139.1143251403882459 ) ) ;
#10553 = CARTESIAN_POINT ( 'NONE',  ( 23.10474973039555024, -52.24929059928630437, 5.564967562786278243 ) ) ;
#10554 = FACE_OUTER_BOUND ( 'NONE', #3451, .T. ) ;
#10555 = EDGE_LOOP ( 'NONE', ( #13798, #868 ) ) ;
#10556 = CARTESIAN_POINT ( 'NONE',  ( 108.0866310645538562, 23.25070940071369563, 139.1143251403882459 ) ) ;
#10557 = EDGE_CURVE ( 'NONE', #6896, #2170, #13482, .T. ) ;
#10558 = EDGE_CURVE ( 'NONE', #11155, #6181, #3627, .T. ) ;
#10559 = EDGE_LOOP ( 'NONE', ( #4194, #9366 ) ) ;
#10560 = CARTESIAN_POINT ( 'NONE',  ( 48.00000000000000000, -2.664535259100377906E-14, 139.1143251403882459 ) ) ;
#10561 = AXIS2_PLACEMENT_3D ( 'NONE', #3791, #5317, #14345 ) ;
#10562 = CARTESIAN_POINT ( 'NONE',  ( 45.17127246049422240, 21.75070940071322667, -33.00000000000012790 ) ) ;
#10563 = VECTOR ( 'NONE', #13406, 1000.000000000000000 ) ;
#10564 = ORIENTED_EDGE ( 'NONE', *, *, #13841, .T. ) ;
#10565 = DIRECTION ( 'NONE',  ( 0.000000000000000000, 0.000000000000000000, 1.000000000000000000 ) ) ;
#10566 = CARTESIAN_POINT ( 'NONE',  ( -11.53791661996513085, -9.438577269332638409, -48.38299871084047510 ) ) ;
#10567 = DIRECTION ( 'NONE',  ( -0.000000000000000000, -0.000000000000000000, 1.000000000000000000 ) ) ;
#10568 = ORIENTED_EDGE ( 'NONE', *, *, #13345, .T. ) ;
#10569 = CARTESIAN_POINT ( 'NONE',  ( 23.47858629692700916, -53.24929059928630437, -6.492462156583981070 ) ) ;
#10570 = FACE_OUTER_BOUND ( 'NONE', #7439, .T. ) ;
#10571 = CARTESIAN_POINT ( 'NONE',  ( 114.6731053250840233, 23.25070940071369563, 13.14990448602692474 ) ) ;
#10572 = CARTESIAN_POINT ( 'NONE',  ( 30.26995075049824990, -61.78874994510989183, 3.497001979624811074 ) ) ;
#10573 = CARTESIAN_POINT ( 'NONE',  ( -24.78493442214762155, -6.766828585132234508, -47.63220435834860922 ) ) ;
#10574 = AXIS2_PLACEMENT_3D ( 'NONE', #4702, #9063, #896 ) ;
#10575 = CIRCLE ( 'NONE', #3439, 0.7892041907098262810 ) ;
#10576 = CARTESIAN_POINT ( 'NONE',  ( 119.1667258010536301, -36.15456035933797807, 56.28371344025898537 ) ) ;
#10577 = ORIENTED_EDGE ( 'NONE', *, *, #753, .F. ) ;
#10578 = DIRECTION ( 'NONE',  ( -0.4848096202550659650, -0.8746197071345573892, 0.000000000000000000 ) ) ;
#10579 = ORIENTED_EDGE ( 'NONE', *, *, #14361, .F. ) ;
#10580 = CARTESIAN_POINT ( 'NONE',  ( 0.000000000000000000, 21.75070940071359615, 139.1143251403882459 ) ) ;
#10581 = CARTESIAN_POINT ( 'NONE',  ( 32.43704918934574977, -59.38916093354929870, -2.764669745501080911 ) ) ;
#10582 = DIRECTION ( 'NONE',  ( -1.156482317317871725E-16, 1.000000000000000000, 0.000000000000000000 ) ) ;
#10583 = DIRECTION ( 'NONE',  ( -0.3255681544665827709, -0.9455185755960711091, 0.000000000000000000 ) ) ;
#10584 = EDGE_CURVE ( 'NONE', #1277, #12382, #12221, .T. ) ;
#10585 =( NAMED_UNIT ( * ) SI_UNIT ( $, .STERADIAN. ) SOLID_ANGLE_UNIT ( ) );
#10586 = CARTESIAN_POINT ( 'NONE',  ( -16.99999999999998579, -2.249290599286303927, 38.00000000000012079 ) ) ;
#10587 = CARTESIAN_POINT ( 'NONE',  ( -25.34903703195771385, -6.790201970332132575, 48.06291368403887532 ) ) ;
#10588 = PLANE ( 'NONE',  #8064 ) ;
#10589 = CARTESIAN_POINT ( 'NONE',  ( 33.37897949129445863, -55.03829860714096611, 2.746682580609041580 ) ) ;
#10590 = VERTEX_POINT ( 'NONE', #12332 ) ;
#10591 = CARTESIAN_POINT ( 'NONE',  ( 54.86190032082818391, 1.721056973166403603, 62.84860122826521689 ) ) ;
#10592 = ORIENTED_EDGE ( 'NONE', *, *, #13833, .T. ) ;
#10593 = CARTESIAN_POINT ( 'NONE',  ( 21.74884261173415467, -85.24929059928631148, 4.000000000000001776 ) ) ;
#10594 = ORIENTED_EDGE ( 'NONE', *, *, #4382, .T. ) ;
#10595 = ORIENTED_EDGE ( 'NONE', *, *, #14963, .T. ) ;
#10596 = CARTESIAN_POINT ( 'NONE',  ( 64.21144059111647096, -11.88561900177543329, 75.86747644619509856 ) ) ;
#10597 = CARTESIAN_POINT ( 'NONE',  ( 23.10474973039556801, -53.24929059928630437, -5.564967562786270250 ) ) ;
#10598 = EDGE_CURVE ( 'NONE', #6506, #14878, #5594, .T. ) ;
#10599 = AXIS2_PLACEMENT_3D ( 'NONE', #9128, #13812, #6970 ) ;
#10600 = B_SPLINE_CURVE_WITH_KNOTS ( 'NONE', 3,
 ( #5679, #2052, #15066, #4591, #3524, #6741 ),
 .UNSPECIFIED., .F., .F.,
 ( 4, 2, 4 ),
 ( 0.000000000000000000, 0.008081365602590071667, 0.01616273120518012252 ),
 .UNSPECIFIED. ) ;
#10601 = CARTESIAN_POINT ( 'NONE',  ( 13.77203033081066685, -67.83931925369924443, -3.638954064322520665 ) ) ;
#10602 = ORIENTED_EDGE ( 'NONE', *, *, #10106, .F. ) ;
#10603 = CARTESIAN_POINT ( 'NONE',  ( 12.36791015745245836, -52.24929059928631148, -3.199931146564426232 ) ) ;
#10604 = CARTESIAN_POINT ( 'NONE',  ( -21.85476584171713199, 5.329050157244537900, 48.50000000000012079 ) ) ;
#10605 = VECTOR ( 'NONE', #6564, 1000.000000000000000 ) ;
#10606 = CARTESIAN_POINT ( 'NONE',  ( 47.27423575335444639, 23.25070940071368852, 84.20452624982236500 ) ) ;
#10607 = ORIENTED_EDGE ( 'NONE', *, *, #15217, .F. ) ;
#10608 = VECTOR ( 'NONE', #13990, 1000.000000000000000 ) ;
#10609 = ORIENTED_EDGE ( 'NONE', *, *, #11615, .F. ) ;
#10610 = CARTESIAN_POINT ( 'NONE',  ( 64.77146624638496064, -11.50114768494419160, 76.78128728924484392 ) ) ;
#10611 = ORIENTED_EDGE ( 'NONE', *, *, #987, .T. ) ;
#10612 = DIRECTION ( 'NONE',  ( -0.000000000000000000, -0.000000000000000000, 1.000000000000000000 ) ) ;
#10613 = EDGE_LOOP ( 'NONE', ( #11963, #13071, #5616, #2372 ) ) ;
#10614 = EDGE_CURVE ( 'NONE', #8444, #11311, #4305, .T. ) ;
#10615 = ORIENTED_EDGE ( 'NONE', *, *, #351, .F. ) ;
#10616 = CARTESIAN_POINT ( 'NONE',  ( -23.19801677984724364, 4.285555568094122414, -47.93908580834070676 ) ) ;
#10617 = DIRECTION ( 'NONE',  ( 0.000000000000000000, 0.000000000000000000, 1.000000000000000000 ) ) ;
#10618 = VERTEX_POINT ( 'NONE', #6484 ) ;
#10619 = AXIS2_PLACEMENT_3D ( 'NONE', #3135, #8908, #12605 ) ;
#10620 = CIRCLE ( 'NONE', #12836, 0.7892041907098290565 ) ;
#10621 = DIRECTION ( 'NONE',  ( 0.000000000000000000, 1.000000000000000000, 4.625929269271485914E-16 ) ) ;
#10622 = CARTESIAN_POINT ( 'NONE',  ( 19.97461805067967333, 0.000000000000000000, 4.000000000000001776 ) ) ;
#10623 = ORIENTED_EDGE ( 'NONE', *, *, #4923, .T. ) ;
#10624 = DIRECTION ( 'NONE',  ( 0.5006040828730989878, -0.8656763553492631269, 0.000000000000000000 ) ) ;
#10625 = CARTESIAN_POINT ( 'NONE',  ( -9.444091399599896519, 2.640528280493846580, -48.24517880332174968 ) ) ;
#10626 = ADVANCED_FACE ( 'NONE', ( #10028 ), #7556, .T. ) ;
#10627 = DIRECTION ( 'NONE',  ( 0.000000000000000000, 0.000000000000000000, 1.000000000000000000 ) ) ;
#10628 = VERTEX_POINT ( 'NONE', #3026 ) ;
#10629 = AXIS2_PLACEMENT_3D ( 'NONE', #679, #12541, #11591 ) ;
#10630 = CYLINDRICAL_SURFACE ( 'NONE', #11245, 0.9999999999999954481 ) ;
#10631 = AXIS2_PLACEMENT_3D ( 'NONE', #9897, #425, #14507 ) ;
#10632 = AXIS2_PLACEMENT_3D ( 'NONE', #12011, #2706, #2784 ) ;
#10633 = ORIENTED_EDGE ( 'NONE', *, *, #7912, .T. ) ;
#10634 = AXIS2_PLACEMENT_3D ( 'NONE', #4276, #13600, #12373 ) ;
#10635 = DIRECTION ( 'NONE',  ( -0.000000000000000000, 0.000000000000000000, -1.000000000000000000 ) ) ;
#10636 = DIRECTION ( 'NONE',  ( 0.000000000000000000, 0.000000000000000000, 1.000000000000000000 ) ) ;
#10637 = ORIENTED_EDGE ( 'NONE', *, *, #3576, .F. ) ;
#10638 = CARTESIAN_POINT ( 'NONE',  ( -2.688903428702175252E-15, 23.25070940071368142, -13.14990448602693007 ) ) ;
#10639 = ADVANCED_FACE ( 'NONE', ( #3871 ), #408, .T. ) ;
#10640 = CARTESIAN_POINT ( 'NONE',  ( 46.91810375148135392, 0.000000000000000000, 33.00000000000012790 ) ) ;
#10641 = ORIENTED_EDGE ( 'NONE', *, *, #9835, .T. ) ;
#10642 = CARTESIAN_POINT ( 'NONE',  ( -9.035163663297472780, 1.943345362497546747, -48.01692658285808335 ) ) ;
#10643 = VECTOR ( 'NONE', #12192, 1000.000000000000000 ) ;
#10644 = CARTESIAN_POINT ( 'NONE',  ( 40.00000000000001421, -74.24929059928631148, -33.00000000000000000 ) ) ;
#10645 = EDGE_CURVE ( 'NONE', #5424, #2756, #4613, .T. ) ;
#10646 = EDGE_CURVE ( 'NONE', #11917, #879, #13633, .T. ) ;
#10647 = EDGE_CURVE ( 'NONE', #1844, #13613, #855, .T. ) ;
#10648 = FACE_OUTER_BOUND ( 'NONE', #5992, .T. ) ;
#10649 = CARTESIAN_POINT ( 'NONE',  ( 58.92629142760364402, 23.25070940071368852, -33.00000000000012790 ) ) ;
#10650 = AXIS2_PLACEMENT_3D ( 'NONE', #6359, #13421, #13288 ) ;
#10651 = CARTESIAN_POINT ( 'NONE',  ( 63.04142083571589694, -2.691337429055927988, 60.61639468829817190 ) ) ;
#10652 = CARTESIAN_POINT ( 'NONE',  ( 32.72652119040196794, -55.34955111272466155, -2.958349455637756531 ) ) ;
#10653 = EDGE_CURVE ( 'NONE', #11350, #14454, #5860, .T. ) ;
#10654 = ORIENTED_EDGE ( 'NONE', *, *, #8512, .T. ) ;
#10655 = DIRECTION ( 'NONE',  ( -1.000000000000000000, 0.000000000000000000, 0.000000000000000000 ) ) ;
#10656 = EDGE_LOOP ( 'NONE', ( #3306, #13997, #15212, #9478 ) ) ;
#10657 = CARTESIAN_POINT ( 'NONE',  ( 9.167948996869769829, -53.67524880067755078, -2.284438283807834758 ) ) ;
#10658 = DIRECTION ( 'NONE',  ( -0.000000000000000000, -1.000000000000000000, -0.000000000000000000 ) ) ;
#10659 = VECTOR ( 'NONE', #14753, 1000.000000000000000 ) ;
#10660 = CARTESIAN_POINT ( 'NONE',  ( 80.00000000000001421, -74.24929059928631148, -32.99999999999999289 ) ) ;
#10661 = DIRECTION ( 'NONE',  ( 0.3020115420618265656, -0.1674077314120193949, 0.9384901064608611732 ) ) ;
#10662 = TOROIDAL_SURFACE ( 'NONE', #5249, 3.694885682588112452, 0.5000000000000000000 ) ;
#10663 = CARTESIAN_POINT ( 'NONE',  ( 70.08913995591909440, -3.527907623570947226, 75.87049022768096052 ) ) ;
#10664 = FILL_AREA_STYLE_COLOUR ( '', #7649 ) ;
#10665 = DIRECTION ( 'NONE',  ( 0.8420378618367644341, 0.5394184268574535590, 0.000000000000000000 ) ) ;
#10666 = LINE ( 'NONE', #8212, #2489 ) ;
#10667 = DIRECTION ( 'NONE',  ( -1.000000000000000000, -0.000000000000000000, -0.000000000000000000 ) ) ;
#10668 = ADVANCED_FACE ( 'NONE', ( #5798 ), #4103, .T. ) ;
#10669 = CARTESIAN_POINT ( 'NONE',  ( 32.60126426873069505, -53.72848551507535575, 3.102677277821895174 ) ) ;
#10670 = AXIS2_PLACEMENT_3D ( 'NONE', #4048, #306, #2609 ) ;
#10671 = ORIENTED_EDGE ( 'NONE', *, *, #6589, .T. ) ;
#10672 = FACE_OUTER_BOUND ( 'NONE', #2059, .T. ) ;
#10673 = ORIENTED_EDGE ( 'NONE', *, *, #10683, .T. ) ;
#10674 = ORIENTED_EDGE ( 'NONE', *, *, #5278, .F. ) ;
#10675 = CARTESIAN_POINT ( 'NONE',  ( 0.000000000000000000, 15.25070940071369563, -33.00000000000012790 ) ) ;
#10676 = ORIENTED_EDGE ( 'NONE', *, *, #7759, .F. ) ;
#10677 = FACE_OUTER_BOUND ( 'NONE', #14354, .T. ) ;
#10678 = CARTESIAN_POINT ( 'NONE',  ( -16.99999999999998579, -2.249290599286303927, -38.50000000000012790 ) ) ;
#10679 = B_SPLINE_CURVE_WITH_KNOTS ( 'NONE', 3,
 ( #14734, #801, #9127, #5515, #5667, #13582, #3347, #8046, #13659, #10200, #13811, #12587, #6731, #3274, #12748, #6575, #7740, #643, #876, #7973, #3117, #2111, #6807 ),
 .UNSPECIFIED., .F., .F.,
 ( 4, 2, 2, 2, 2, 2, 2, 1, 2, 2, 2, 4 ),
 ( 0.000000000000000000, 0.0009744059347753146819, 0.001948811869550629364, 0.002436014836938296679, 0.002923217804325963995, 0.003897623739101298626, 0.004384826706488958135, 0.004872029673876616777, 0.005359232641264276287, 0.005846435608651934061, 0.006820841543427254815, 0.007795247478202574701 ),
 .UNSPECIFIED. ) ;
#10680 = LINE ( 'NONE', #2441, #1303 ) ;
#10681 = CARTESIAN_POINT ( 'NONE',  ( 9.351153736313083442, -54.69057383520976856, 3.126673503084359318 ) ) ;
#10682 = DIRECTION ( 'NONE',  ( 1.156482317317870492E-16, -1.000000000000000000, 0.000000000000000000 ) ) ;
#10683 = EDGE_CURVE ( 'NONE', #4458, #5141, #14862, .T. ) ;
#10684 = EDGE_CURVE ( 'NONE', #13307, #5064, #1416, .T. ) ;
#10685 = CYLINDRICAL_SURFACE ( 'NONE', #1409, 9.000000000000001776 ) ;
#10686 = ORIENTED_EDGE ( 'NONE', *, *, #6494, .F. ) ;
#10687 = ORIENTED_EDGE ( 'NONE', *, *, #6273, .F. ) ;
#10688 = CARTESIAN_POINT ( 'NONE',  ( -6.999999999999985789, -2.249290599286299930, 33.00000000000012790 ) ) ;
#10689 = ORIENTED_EDGE ( 'NONE', *, *, #10963, .T. ) ;
#10690 = ORIENTED_EDGE ( 'NONE', *, *, #9567, .F. ) ;
#10691 = CARTESIAN_POINT ( 'NONE',  ( 9.665751080312901422, -60.12777237996191104, -2.859594828286806667 ) ) ;
#10692 = EDGE_LOOP ( 'NONE', ( #2610, #11988, #6661, #7992 ) ) ;
#10693 = CARTESIAN_POINT ( 'NONE',  ( 27.79575038568464151, -66.12098470289355134, 4.407543342774871142 ) ) ;
#10694 = EDGE_LOOP ( 'NONE', ( #10367, #2141, #14779, #14136 ) ) ;
#10695 = CARTESIAN_POINT ( 'NONE',  ( -24.34228330361342785, 2.967490118658024034, -47.54143911729025973 ) ) ;
#10696 = DIRECTION ( 'NONE',  ( 0.000000000000000000, 1.000000000000000000, 0.000000000000000000 ) ) ;
#10697 = ORIENTED_EDGE ( 'NONE', *, *, #11766, .T. ) ;
#10698 = DIRECTION ( 'NONE',  ( -0.8381289428352193260, -0.5454721580263449665, 0.000000000000000000 ) ) ;
#10699 = LINE ( 'NONE', #14089, #7424 ) ;
#10700 = ORIENTED_EDGE ( 'NONE', *, *, #9079, .T. ) ;
#10701 = EDGE_CURVE ( 'NONE', #3972, #9345, #15026, .T. ) ;
#10702 = CARTESIAN_POINT ( 'NONE',  ( -2.688903428702175252E-15, 23.25070940071368142, 33.00000000000012790 ) ) ;
#10703 = CARTESIAN_POINT ( 'NONE',  ( -24.54316048551696028, -7.158540021523408292, 48.50000000000012079 ) ) ;
#10704 = EDGE_CURVE ( 'NONE', #1441, #6995, #10414, .T. ) ;
#10705 = CARTESIAN_POINT ( 'NONE',  ( -16.99999999999998579, -2.249290599286303927, 50.00000000000012079 ) ) ;
#10706 = ORIENTED_EDGE ( 'NONE', *, *, #6533, .F. ) ;
#10707 = ADVANCED_BREP_SHAPE_REPRESENTATION ( '', ( #14171, #6315 ), #3366 ) ;
#10708 = CARTESIAN_POINT ( 'NONE',  ( 65.92402464212069901, -2.249290599286309256, 38.50000000000012790 ) ) ;
#10709 = ORIENTED_EDGE ( 'NONE', *, *, #11615, .T. ) ;
#10710 = CARTESIAN_POINT ( 'NONE',  ( 58.00000000000000711, -2.249290599286309256, 71.19766410831374515 ) ) ;
#10711 =( NAMED_UNIT ( * ) SI_UNIT ( $, .STERADIAN. ) SOLID_ANGLE_UNIT ( ) );
#10712 = VERTEX_POINT ( 'NONE', #4312 ) ;
#10713 = CARTESIAN_POINT ( 'NONE',  ( -12.14523415828302078, -9.827631355817260328, -48.50000000000012079 ) ) ;
#10714 = CARTESIAN_POINT ( 'NONE',  ( 32.39917484285220439, 0.000000000000000000, 139.1143251403882459 ) ) ;
#10715 = CARTESIAN_POINT ( 'NONE',  ( -9.443282642412393457, 2.639297360524499592, -48.23807154671105479 ) ) ;
#10716 = CIRCLE ( 'NONE', #9746, 3.999999999999999112 ) ;
#10717 = CARTESIAN_POINT ( 'NONE',  ( 20.86173033120691045, -96.56299909827106376, 3.999999999999999112 ) ) ;
#10718 = DIRECTION ( 'NONE',  ( 1.000000000000000000, 0.000000000000000000, 0.000000000000000000 ) ) ;
#10719 = CARTESIAN_POINT ( 'NONE',  ( 27.69308748103538775, -66.48338622332397563, 4.442552071294104898 ) ) ;
#10720 = LINE ( 'NONE', #12104, #86 ) ;
#10721 = CARTESIAN_POINT ( 'NONE',  ( 30.59224152647144024, -52.42016302384283222, -2.859972208321964970 ) ) ;
#10722 = EDGE_CURVE ( 'NONE', #8760, #9351, #4872, .T. ) ;
#10723 = ORIENTED_EDGE ( 'NONE', *, *, #14642, .T. ) ;
#10724 = CIRCLE ( 'NONE', #15148, 6.000000000000000000 ) ;
#10725 = DIRECTION ( 'NONE',  ( -0.000000000000000000, -1.000000000000000000, -0.000000000000000000 ) ) ;
#10726 = ORIENTED_EDGE ( 'NONE', *, *, #9176, .F. ) ;
#10727 = DIRECTION ( 'NONE',  ( -1.000000000000000000, 0.000000000000000000, 0.000000000000000000 ) ) ;
#10728 = CARTESIAN_POINT ( 'NONE',  ( 103.2469880950108063, 21.75070940071363168, 33.00000000000012790 ) ) ;
#10729 = CYLINDRICAL_SURFACE ( 'NONE', #2537, 0.5000000000000000000 ) ;
#10730 = DIRECTION ( 'NONE',  ( -0.000000000000000000, -0.000000000000000000, -1.000000000000000000 ) ) ;
#10731 = DIRECTION ( 'NONE',  ( 0.000000000000000000, 0.000000000000000000, 1.000000000000000000 ) ) ;
#10732 = CARTESIAN_POINT ( 'NONE',  ( 64.94561305207867008, -11.37113100889128248, 71.46833336701176620 ) ) ;
#10733 = EDGE_CURVE ( 'NONE', #7249, #14177, #9790, .T. ) ;
#10734 = CIRCLE ( 'NONE', #15158, 0.5000000000000004441 ) ;
#10735 = AXIS2_PLACEMENT_3D ( 'NONE', #5196, #2966, #5276 ) ;
#10736 = CARTESIAN_POINT ( 'NONE',  ( 96.00000000000002842, 6.750709400713692965, 33.00000000000012790 ) ) ;
#10737 = CARTESIAN_POINT ( 'NONE',  ( -24.96151347116557062, -6.448033549061094938, 47.50000000626571506 ) ) ;
#10738 = CIRCLE ( 'NONE', #13201, 4.194885682588113340 ) ;
#10739 = CARTESIAN_POINT ( 'NONE',  ( 31.72224702437784316, -52.94991738523431479, 2.538129127160420051 ) ) ;
#10740 =( GEOMETRIC_REPRESENTATION_CONTEXT ( 3 ) GLOBAL_UNCERTAINTY_ASSIGNED_CONTEXT ( ( #1505 ) ) GLOBAL_UNIT_ASSIGNED_CONTEXT ( ( #623, #10329, #7718 ) ) REPRESENTATION_CONTEXT ( 'NONE', 'WORKASPACE' ) );
#10741 = VERTEX_POINT ( 'NONE', #3322 ) ;
#10742 = DIRECTION ( 'NONE',  ( 0.5006040828730401460, -0.8656763553492970997, 0.000000000000000000 ) ) ;
#10743 = EDGE_LOOP ( 'NONE', ( #6485, #8251, #565, #11814 ) ) ;
#10744 = EDGE_CURVE ( 'NONE', #5398, #12776, #11394, .T. ) ;
#10745 = CARTESIAN_POINT ( 'NONE',  ( 8.333746545461773181, -58.06117555224668081, 1.821720187977012628 ) ) ;
#10746 = VECTOR ( 'NONE', #3659, 1000.000000000000000 ) ;
#10747 = EDGE_LOOP ( 'NONE', ( #14619, #5556, #14096, #269 ) ) ;
#10748 = EDGE_CURVE ( 'NONE', #11670, #15071, #10253, .T. ) ;
#10749 = AXIS2_PLACEMENT_3D ( 'NONE', #12656, #3271, #13887 ) ;
#10750 = EDGE_LOOP ( 'NONE', ( #7279, #8370, #4992, #4022 ) ) ;
#10751 = CARTESIAN_POINT ( 'NONE',  ( 65.71319926014257362, -10.73129157630437014, 76.19766410831375936 ) ) ;
#10752 = DIRECTION ( 'NONE',  ( -1.000000000000000000, 0.000000000000000000, 0.000000000000000000 ) ) ;
#10753 = DIRECTION ( 'NONE',  ( -1.000000000000000000, 0.000000000000000000, 0.000000000000000000 ) ) ;
#10754 = AXIS2_PLACEMENT_3D ( 'NONE', #5774, #15225, #824 ) ;
#10755 = CARTESIAN_POINT ( 'NONE',  ( 8.766647633345350243, -57.08478275174014271, 2.747861298827293908 ) ) ;
#10756 = AXIS2_PLACEMENT_3D ( 'NONE', #15092, #3546, #4541 ) ;
#10757 = AXIS2_PLACEMENT_3D ( 'NONE', #8764, #13322, #8696 ) ;
#10758 = FACE_BOUND ( 'NONE', #3456, .T. ) ;
#10759 = DIRECTION ( 'NONE',  ( 0.8746197071345560570, -0.4848096202550682410, 0.000000000000000000 ) ) ;
#10760 = ORIENTED_EDGE ( 'NONE', *, *, #3385, .F. ) ;
#10761 = ORIENTED_EDGE ( 'NONE', *, *, #1969, .T. ) ;
#10762 = DIRECTION ( 'NONE',  ( -0.8656763553492639041, -0.5006040828730973224, 0.000000000000000000 ) ) ;
#10763 = EDGE_LOOP ( 'NONE', ( #11294, #14751 ) ) ;
#10764 = CARTESIAN_POINT ( 'NONE',  ( 58.00000000000000711, -2.249290599286309256, 86.40005259842790508 ) ) ;
#10765 = VECTOR ( 'NONE', #5133, 1000.000000000000000 ) ;
#10766 = ORIENTED_EDGE ( 'NONE', *, *, #11531, .T. ) ;
#10767 = DIRECTION ( 'NONE',  ( 1.000000000000000000, 0.000000000000000000, 0.000000000000000000 ) ) ;
#10768 = ORIENTED_EDGE ( 'NONE', *, *, #11339, .T. ) ;
#10769 = VECTOR ( 'NONE', #197, 1000.000000000000000 ) ;
#10770 = AXIS2_PLACEMENT_3D ( 'NONE', #13769, #12692, #4221 ) ;
#10771 = CARTESIAN_POINT ( 'NONE',  ( 40.00000000000001421, 23.95881716715930665, -32.99999999999982947 ) ) ;
#10772 = CARTESIAN_POINT ( 'NONE',  ( 69.44738493598792672, -2.877909345519603868, 73.19766410831374515 ) ) ;
#10773 = VERTEX_POINT ( 'NONE', #6781 ) ;
#10774 = EDGE_CURVE ( 'NONE', #6522, #7200, #6825, .T. ) ;
#10775 = DIRECTION ( 'NONE',  ( -0.5454721580263448555, 0.8381289428352193260, 0.000000000000000000 ) ) ;
#10776 = LINE ( 'NONE', #236, #13320 ) ;
#10777 = VERTEX_POINT ( 'NONE', #14945 ) ;
#10778 = EDGE_CURVE ( 'NONE', #10074, #13054, #4553, .T. ) ;
#10779 = TOROIDAL_SURFACE ( 'NONE', #6115, 3.999999999999996447, 1.000000000000000000 ) ;
#10780 = LINE ( 'NONE', #4928, #942 ) ;
#10781 = CARTESIAN_POINT ( 'NONE',  ( -9.358536206588548012, 2.506280377409947135, -47.89606589046130125 ) ) ;
#10782 = FACE_OUTER_BOUND ( 'NONE', #8551, .T. ) ;
#10783 = AXIS2_PLACEMENT_3D ( 'NONE', #10586, #4659, #3428 ) ;
#10784 = EDGE_LOOP ( 'NONE', ( #12496, #4140, #2513, #7292 ) ) ;
#10785 = FACE_OUTER_BOUND ( 'NONE', #11064, .T. ) ;
#10786 = EDGE_LOOP ( 'NONE', ( #2646, #13842, #4216, #8553 ) ) ;
#10787 = CARTESIAN_POINT ( 'NONE',  ( 48.00000000000000000, -2.249290599286307479, -33.00000000000012790 ) ) ;
#10788 = DIRECTION ( 'NONE',  ( 1.000000000000000000, 0.000000000000000000, 0.000000000000000000 ) ) ;
#10789 = ORIENTED_EDGE ( 'NONE', *, *, #7384, .F. ) ;
#10790 = ADVANCED_FACE ( 'NONE', ( #6943 ), #1462, .F. ) ;
#10791 = SHAPE_DEFINITION_REPRESENTATION ( #12488, #1557 ) ;
#10792 = PLANE ( 'NONE',  #3381 ) ;
#10793 = CARTESIAN_POINT ( 'NONE',  ( 24.10826840236108737, -69.39711819508849544, 6.201611931792130328 ) ) ;
#10794 = EDGE_CURVE ( 'NONE', #11647, #5697, #14257, .T. ) ;
#10795 = PLANE ( 'NONE',  #11192 ) ;
#10796 = CARTESIAN_POINT ( 'NONE',  ( 17.58146340911564920, -70.03159917004852275, 6.184016381206977719 ) ) ;
#10797 = AXIS2_PLACEMENT_3D ( 'NONE', #1307, #90, #11619 ) ;
#10798 = LINE ( 'NONE', #11870, #7563 ) ;
#10799 = PLANE ( 'NONE',  #3425 ) ;
#10800 = DIRECTION ( 'NONE',  ( 0.000000000000000000, 1.000000000000000000, -0.000000000000000000 ) ) ;
#10801 = CARTESIAN_POINT ( 'NONE',  ( 33.42858924011148503, -55.21335607387715783, -1.971947758011750595 ) ) ;
#10802 = VECTOR ( 'NONE', #29, 1000.000000000000000 ) ;
#10803 = AXIS2_PLACEMENT_3D ( 'NONE', #10262, #4403, #11178 ) ;
#10804 = LINE ( 'NONE', #263, #11539 ) ;
#10805 = ORIENTED_EDGE ( 'NONE', *, *, #14266, .F. ) ;
#10806 = CARTESIAN_POINT ( 'NONE',  ( 32.48672609961973734, -59.22985212983979153, -2.757908476812882093 ) ) ;
#10807 = ADVANCED_FACE ( 'NONE', ( #14182 ), #1166, .T. ) ;
#10808 = SHAPE_REPRESENTATION_RELATIONSHIP ( 'NONE' , 'NONE' ,  #2630, #11812 ) ;
#10809 = DIRECTION ( 'NONE',  ( 0.8656763553493062036, 0.5006040828730242698, -0.000000000000000000 ) ) ;
#10810 = CARTESIAN_POINT ( 'NONE',  ( 114.6731053250840233, 23.25070940071369563, -13.14990448602692474 ) ) ;
#10811 = DIRECTION ( 'NONE',  ( -0.8420378618367644341, -0.5394184268574535590, -0.000000000000000000 ) ) ;
#10812 = VECTOR ( 'NONE', #13394, 1000.000000000000000 ) ;
#10813 = AXIS2_PLACEMENT_3D ( 'NONE', #10498, #10725, #2572 ) ;
#10814 = CARTESIAN_POINT ( 'NONE',  ( 70.05014002589594213, -3.391651902948124242, 75.75351273523833129 ) ) ;
#10815 = DIRECTION ( 'NONE',  ( 0.000000000000000000, 0.000000000000000000, -1.000000000000000000 ) ) ;
#10816 = CARTESIAN_POINT ( 'NONE',  ( 33.10838500789091654, -54.46933172536108714, 2.097670533078143329 ) ) ;
#10817 = VERTEX_POINT ( 'NONE', #7099 ) ;
#10818 = CARTESIAN_POINT ( 'NONE',  ( 100.0000000000000284, 0.000000000000000000, -33.00000000000012790 ) ) ;
#10819 = ORIENTED_EDGE ( 'NONE', *, *, #2181, .F. ) ;
#10820 = ADVANCED_FACE ( 'NONE', ( #8490 ), #3636, .F. ) ;
#10821 = DIRECTION ( 'NONE',  ( 0.000000000000000000, -1.000000000000000000, -1.927470528863119788E-16 ) ) ;
#10822 = AXIS2_PLACEMENT_3D ( 'NONE', #5291, #7750, #8898 ) ;
#10823 = ORIENTED_EDGE ( 'NONE', *, *, #3952, .F. ) ;
#10825 = ORIENTED_EDGE ( 'NONE', *, *, #6298, .T. ) ;
#10824 = CARTESIAN_POINT ( 'NONE',  ( 64.34994344588844228, -11.79539688520061702, 76.23544073996576742 ) ) ;
#10826 = DIRECTION ( 'NONE',  ( -0.000000000000000000, -0.000000000000000000, 1.000000000000000000 ) ) ;
#10827 = DIRECTION ( 'NONE',  ( 0.000000000000000000, -1.000000000000000000, 0.000000000000000000 ) ) ;
#10828 = ORIENTED_EDGE ( 'NONE', *, *, #431, .F. ) ;
#10829 = CARTESIAN_POINT ( 'NONE',  ( 8.408558643351286221, -54.89597349494646750, 2.779010397565546242 ) ) ;
#10830 = ADVANCED_FACE ( 'NONE', ( #7322 ), #10792, .F. ) ;
#10831 = CIRCLE ( 'NONE', #14749, 0.7892041907098262810 ) ;
#10832 = EDGE_CURVE ( 'NONE', #14864, #6792, #5881, .T. ) ;
#10833 = DIRECTION ( 'NONE',  ( -0.8420378618367728718, -0.5394184268574404584, 0.000000000000000000 ) ) ;
#10834 = FACE_OUTER_BOUND ( 'NONE', #6022, .T. ) ;
#10835 = ORIENTED_EDGE ( 'NONE', *, *, #5807, .T. ) ;
#10836 = VERTEX_POINT ( 'NONE', #8413 ) ;
#10837 = DIRECTION ( 'NONE',  ( -0.005897974685767391929, 0.9999826067960413400, 0.000000000000000000 ) ) ;
#10838 = ORIENTED_EDGE ( 'NONE', *, *, #7752, .F. ) ;
#10839 = ADVANCED_FACE ( 'NONE', ( #11785 ), #2561, .T. ) ;
#10840 = CARTESIAN_POINT ( 'NONE',  ( 11.45230383124209617, -61.78784708351296473, 3.496562482608114308 ) ) ;
#10841 = EDGE_LOOP ( 'NONE', ( #7476, #8378, #15004, #14690 ) ) ;
#10842 = ORIENTED_EDGE ( 'NONE', *, *, #15217, .T. ) ;
#10843 = CARTESIAN_POINT ( 'NONE',  ( 56.97758043373130477, 2.707118148285912795, 48.51982618741349285 ) ) ;
#10844 = AXIS2_PLACEMENT_3D ( 'NONE', #488, #6411, #10031 ) ;
#10845 = ORIENTED_EDGE ( 'NONE', *, *, #1194, .T. ) ;
#10846 = DIRECTION ( 'NONE',  ( -0.3020115420618285085, 0.1674077314120178406, -0.9384901064608609511 ) ) ;
#10847 = DIRECTION ( 'NONE',  ( 0.000000000000000000, -1.000000000000000000, 0.000000000000000000 ) ) ;
#10848 = ORIENTED_EDGE ( 'NONE', *, *, #5512, .F. ) ;
#10849 = ADVANCED_FACE ( 'NONE', ( #7172 ), #14710, .T. ) ;
#10850 = LINE ( 'NONE', #3464, #2748 ) ;
#10851 = FACE_OUTER_BOUND ( 'NONE', #3833, .T. ) ;
#10852 = CIRCLE ( 'NONE', #4190, 2.000000000000000000 ) ;
#10853 = VERTEX_POINT ( 'NONE', #13029 ) ;
#10854 = CIRCLE ( 'NONE', #760, 0.7892041907098278353 ) ;
#10855 = CARTESIAN_POINT ( 'NONE',  ( -80.00000000000001421, -74.24929059928631148, -32.99999999999999289 ) ) ;
#10856 = CARTESIAN_POINT ( 'NONE',  ( 32.52281604437752804, -59.06479067038043240, 2.757123406423070744 ) ) ;
#10857 = DIRECTION ( 'NONE',  ( -0.000000000000000000, 1.000000000000000000, 1.445602896647339163E-16 ) ) ;
#10858 = ORIENTED_EDGE ( 'NONE', *, *, #7970, .T. ) ;
#10859 = CYLINDRICAL_SURFACE ( 'NONE', #13232, 4.000000000000003553 ) ;
#10860 = EDGE_CURVE ( 'NONE', #13513, #14513, #172, .T. ) ;
#10861 = ORIENTED_EDGE ( 'NONE', *, *, #10778, .T. ) ;
#10862 = CIRCLE ( 'NONE', #12565, 0.5000000000000001110 ) ;
#10863 = ORIENTED_EDGE ( 'NONE', *, *, #9501, .F. ) ;
#10864 = CIRCLE ( 'NONE', #10619, 2.500000000000002220 ) ;
#10865 = DIRECTION ( 'NONE',  ( -1.000000000000000000, 0.000000000000000000, 0.000000000000000000 ) ) ;
#10866 = CARTESIAN_POINT ( 'NONE',  ( 69.28051765693513175, -4.295678830383772961, 71.19766410831374515 ) ) ;
#10867 = VERTEX_POINT ( 'NONE', #4864 ) ;
#10868 = APPLICATION_PROTOCOL_DEFINITION ( 'draft international standard', 'automotive_design', 1998, #11431 ) ;
#10869 = CARTESIAN_POINT ( 'NONE',  ( -12.99999999999998757, -2.249290599286303927, -38.00000000000012079 ) ) ;
#10870 = CARTESIAN_POINT ( 'NONE',  ( 96.29968967959054282, 25.52935533987996664, -33.00000000000012790 ) ) ;
#10871 = CARTESIAN_POINT ( 'NONE',  ( 9.696105087471012851, 30.24276591118031021, 0.000000000000000000 ) ) ;
#10872 = ORIENTED_EDGE ( 'NONE', *, *, #10645, .F. ) ;
#10873 = CARTESIAN_POINT ( 'NONE',  ( 6.633218499801108337, -47.02718879221286841, 2.731995254387804106 ) ) ;
#10874 = LINE ( 'NONE', #14412, #9282 ) ;
#10876 = CARTESIAN_POINT ( 'NONE',  ( 0.000000000000000000, 21.75070940071369918, 13.14990448602693007 ) ) ;
#10875 =( REPRESENTATION_RELATIONSHIP ('NONE','NONE', #15125, #3114 ) REPRESENTATION_RELATIONSHIP_WITH_TRANSFORMATION ( #8843 )SHAPE_REPRESENTATION_RELATIONSHIP( ) );
#10877 = FACE_OUTER_BOUND ( 'NONE', #5728, .T. ) ;
#10878 = AXIS2_PLACEMENT_3D ( 'NONE', #11329, #793, #10194 ) ;
#10879 = CARTESIAN_POINT ( 'NONE',  ( -24.54316048551696383, -7.158540021523408292, 48.37147253714708484 ) ) ;
#10880 = CARTESIAN_POINT ( 'NONE',  ( 32.81365369610337979, -55.58532807872790471, -2.910983838681297620 ) ) ;
#10881 = CIRCLE ( 'NONE', #9669, 0.5000000000000004441 ) ;
#10882 = ADVANCED_FACE ( 'NONE', ( #13172 ), #2628, .T. ) ;
#10883 = ADVANCED_FACE ( 'NONE', ( #11016 ), #193, .T. ) ;
#10884 = ORIENTED_EDGE ( 'NONE', *, *, #11367, .T. ) ;
#10885 = CARTESIAN_POINT ( 'NONE',  ( 100.0000000000000284, 0.000000000000000000, 139.1143251403882459 ) ) ;
#10886 = CARTESIAN_POINT ( 'NONE',  ( 32.54790116764300478, -57.26105658658105568, -1.816685854991389348 ) ) ;
#10887 = CIRCLE ( 'NONE', #4479, 2.500000000000002220 ) ;
#10888 =( NAMED_UNIT ( * ) SI_UNIT ( $, .STERADIAN. ) SOLID_ANGLE_UNIT ( ) );
#10889 = CARTESIAN_POINT ( 'NONE',  ( -21.85476584171713199, 5.329050157244537900, -48.50000000000012079 ) ) ;
#10890 = VECTOR ( 'NONE', #4536, 1000.000000000000000 ) ;
#10891 = CARTESIAN_POINT ( 'NONE',  ( 69.39844472759932614, -3.556430582623343550, 76.16265406106171554 ) ) ;
#10892 = CARTESIAN_POINT ( 'NONE',  ( 68.00000000000000000, 2.750709400713692965, 33.00000000000012790 ) ) ;
#10893 = CARTESIAN_POINT ( 'NONE',  ( 65.43388225677183812, -11.84036758951991963, 72.57413203708259175 ) ) ;
#10894 = DIRECTION ( 'NONE',  ( -1.000000000000000000, -1.110223024625156540E-15, 0.000000000000000000 ) ) ;
#10895 = DIRECTION ( 'NONE',  ( 1.000000000000000000, 0.000000000000000000, 0.000000000000000000 ) ) ;
#10896 = ADVANCED_FACE ( 'NONE', ( #9795 ), #438, .F. ) ;
#10897 = EDGE_CURVE ( 'NONE', #11609, #6596, #9286, .T. ) ;
#10898 = CARTESIAN_POINT ( 'NONE',  ( 70.04068982727432058, -3.360887980114144025, 72.67877579342776073 ) ) ;
#10899 = ORIENTED_EDGE ( 'NONE', *, *, #10946, .F. ) ;
#10900 = CIRCLE ( 'NONE', #12619, 0.7892041907098262810 ) ;
#10901 = DIRECTION ( 'NONE',  ( 0.000000000000000000, -1.000000000000000000, 1.445602896647339410E-16 ) ) ;
#10902 = VECTOR ( 'NONE', #1466, 1000.000000000000000 ) ;
#10903 = ORIENTED_EDGE ( 'NONE', *, *, #7106, .T. ) ;
#10904 = CARTESIAN_POINT ( 'NONE',  ( 16.53849081582479741, -69.39711819508849544, -5.637959728397558656 ) ) ;
#10905 = VERTEX_POINT ( 'NONE', #14480 ) ;
#10906 = VERTEX_POINT ( 'NONE', #13254 ) ;
#10908 = VERTEX_POINT ( 'NONE', #7621 ) ;
#10907 = PLANE ( 'NONE',  #9666 ) ;
#10909 = DIRECTION ( 'NONE',  ( 0.000000000000000000, 0.000000000000000000, 1.000000000000000000 ) ) ;
#10910 =( BOUNDED_SURFACE ( )  B_SPLINE_SURFACE ( 3, 2, ( 
 ( #2995, #11148, #7687 ),
 ( #11213, #668, #10071 ),
 ( #14752, #4208, #2297 ),
 ( #13991, #9301, #9225 ),
 ( #972, #4439, #5533 ),
 ( #8067, #1059, #6989 ),
 ( #2135, #13758, #12767 ),
 ( #5686, #11679, #2214 ),
 ( #10218, #3139, #6674 ),
 ( #5453, #13838, #4524 ),
 ( #10377, #13909, #3448 ),
 ( #12610, #11360, #3213 ),
 ( #6828, #7918, #1974 ),
 ( #6906, #822, #2061 ),
 ( #12850, #9153, #897 ),
 ( #11514, #3370, #6748 ),
 ( #5772, #10147, #11598 ),
 ( #11433, #10453, #3294 ),
 ( #14835, #15144, #15076 ),
 ( #14905, #4599, #7838 ),
 ( #7989, #4281, #8982 ),
 ( #8142, #5609, #13680 ),
 ( #12531, #4366, #9064 ),
 ( #10301, #14992, #12683 ) ),
 .UNSPECIFIED., .F., .F., .F. ) 
 B_SPLINE_SURFACE_WITH_KNOTS ( ( 4, 2, 2, 2, 2, 2, 2, 2, 2, 2, 2, 4 ),
 ( 3, 3 ),
 ( 0.000000000000000000, 0.0007569831467696874674, 0.001513966293539374935, 0.002270949440309062185, 0.002649441013693906027, 0.003027932587078749870, 0.003406424160463593712, 0.003784915733848437120, 0.004541898880618124371, 0.004920390454002968213, 0.005298882027387812055, 0.006055865174157499739 ),
 ( 0.000000000000000000, 1.000000000000000000 ),
 .UNSPECIFIED. ) 
 GEOMETRIC_REPRESENTATION_ITEM ( )  RATIONAL_B_SPLINE_SURFACE ( (
 ( 1.000000000000000000, 0.6947298545087537969, 1.000000000000000000),
 ( 1.000000000000000000, 0.7030359819960353418, 1.000000000000000000),
 ( 1.000000000000000000, 0.7110141033721660841, 1.000000000000000000),
 ( 1.000000000000000000, 0.7265357204475634267, 1.000000000000000000),
 ( 1.000000000000000000, 0.7341632328269016572, 1.000000000000000000),
 ( 1.000000000000000000, 0.7486333683862642641, 1.000000000000000000),
 ( 1.000000000000000000, 0.7555062062384456656, 1.000000000000000000),
 ( 1.000000000000000000, 0.7654404118660548262, 1.000000000000000000),
 ( 1.000000000000000000, 0.7687038416332773183, 1.000000000000000000),
 ( 1.000000000000000000, 0.7749762558334875040, 1.000000000000000000),
 ( 1.000000000000000000, 0.7780012814122965192, 1.000000000000000000),
 ( 1.000000000000000000, 0.7838538191795068055, 1.000000000000000000),
 ( 1.000000000000000000, 0.7866813202764467716, 1.000000000000000000),
 ( 1.000000000000000000, 0.7921509987295783928, 1.000000000000000000),
 ( 1.000000000000000000, 0.7948100380743099436, 1.000000000000000000),
 ( 1.000000000000000000, 0.8023666703952255785, 1.000000000000000000),
 ( 1.000000000000000000, 0.8068432255864165237, 1.000000000000000000),
 ( 1.000000000000000000, 0.8126963150101534916, 1.000000000000000000),
 ( 1.000000000000000000, 0.8145123882374375457, 1.000000000000000000),
 ( 1.000000000000000000, 0.8177588193891082158, 1.000000000000000000),
 ( 1.000000000000000000, 0.8191832667250865674, 1.000000000000000000),
 ( 1.000000000000000000, 0.8228396104941049227, 1.000000000000000000),
 ( 1.000000000000000000, 0.8244610879124181224, 1.000000000000000000),
 ( 1.000000000000000000, 0.8250833044923663318, 1.000000000000000000) ) ) 
 REPRESENTATION_ITEM ( '' )  SURFACE ( )  );
#10911 = DIRECTION ( 'NONE',  ( 1.000000000000000000, 0.000000000000000000, 0.000000000000000000 ) ) ;
#10912 = VERTEX_POINT ( 'NONE', #8621 ) ;
#10913 = AXIS2_PLACEMENT_3D ( 'NONE', #10202, #13508, #12589 ) ;
#10914 = CARTESIAN_POINT ( 'NONE',  ( 8.294871422301858033, -55.21335607387847944, 1.971947758013492535 ) ) ;
#10915 = DIRECTION ( 'NONE',  ( -1.000000000000000000, 0.000000000000000000, 0.000000000000000000 ) ) ;
#10916 = DIRECTION ( 'NONE',  ( -1.000000000000000000, 0.000000000000000000, 0.000000000000000000 ) ) ;
#10917 = EDGE_LOOP ( 'NONE', ( #13003, #4604, #10931, #10136 ) ) ;
#10918 = ORIENTED_EDGE ( 'NONE', *, *, #13099, .T. ) ;
#10919 = DIRECTION ( 'NONE',  ( -0.8746197071345572782, 0.4848096202550659650, 0.000000000000000000 ) ) ;
#10920 = ADVANCED_FACE ( 'NONE', ( #6323 ), #14615, .F. ) ;
#10921 = ORIENTED_EDGE ( 'NONE', *, *, #7904, .T. ) ;
#10922 = ORIENTED_EDGE ( 'NONE', *, *, #1858, .T. ) ;
#10923 = DIRECTION ( 'NONE',  ( 0.000000000000000000, 0.000000000000000000, -1.000000000000000000 ) ) ;
#10924 = VERTEX_POINT ( 'NONE', #5163 ) ;
#10925 = CARTESIAN_POINT ( 'NONE',  ( -3.190546569013415379, 0.8906624217387615339, -48.50000000000012079 ) ) ;
#10926 = VERTEX_POINT ( 'NONE', #13537 ) ;
#10927 = EDGE_CURVE ( 'NONE', #2517, #15191, #6389, .T. ) ;
#10928 = EDGE_CURVE ( 'NONE', #1582, #153, #11977, .T. ) ;
#10929 = LINE ( 'NONE', #452, #11211 ) ;
#10930 = DIRECTION ( 'NONE',  ( 0.000000000000000000, 1.000000000000000000, -0.000000000000000000 ) ) ;
#10931 = ORIENTED_EDGE ( 'NONE', *, *, #1721, .T. ) ;
#10932 = CYLINDRICAL_SURFACE ( 'NONE', #8161, 0.4999999999999996669 ) ;
#10933 = EDGE_LOOP ( 'NONE', ( #1435, #7977 ) ) ;
#10934 = ADVANCED_FACE ( 'NONE', ( #535 ), #9868, .F. ) ;
#10935 = EDGE_CURVE ( 'NONE', #5660, #10628, #6566, .T. ) ;
#10936 = CARTESIAN_POINT ( 'NONE',  ( 42.07846078193830408, 21.75070940071319114, 33.00000000000012790 ) ) ;
#10937 = DIRECTION ( 'NONE',  ( 0.000000000000000000, 0.000000000000000000, -1.000000000000000000 ) ) ;
#10938 = CARTESIAN_POINT ( 'NONE',  ( -3.190546569013415379, 0.8906624217387615339, 48.00000000000012079 ) ) ;
#10939 = ORIENTED_EDGE ( 'NONE', *, *, #7268, .F. ) ;
#10940 = DIRECTION ( 'NONE',  ( -0.000000000000000000, -0.000000000000000000, -1.000000000000000000 ) ) ;
#10941 = ADVANCED_FACE ( 'NONE', ( #2783 ), #2844, .T. ) ;
#10942 = VERTEX_POINT ( 'NONE', #3007 ) ;
#10943 = EDGE_CURVE ( 'NONE', #943, #3036, #6098, .T. ) ;
#10944 = CARTESIAN_POINT ( 'NONE',  ( 116.6234642359097222, -39.31822372505217089, 54.40673322733726991 ) ) ;
#10945 = ORIENTED_EDGE ( 'NONE', *, *, #1603, .T. ) ;
#10946 = EDGE_CURVE ( 'NONE', #4644, #2314, #14407, .T. ) ;
#10947 = SHAPE_DEFINITION_REPRESENTATION ( #4244, #2449 ) ;
#10948 = DIRECTION ( 'NONE',  ( -0.000000000000000000, -0.000000000000000000, -1.000000000000000000 ) ) ;
#10949 = CARTESIAN_POINT ( 'NONE',  ( 104.9938193859979236, 21.75070940071363168, -33.00000000000012790 ) ) ;
#10950 = CARTESIAN_POINT ( 'NONE',  ( 64.90552635791956959, 22.43695620243006772, 84.20452624982236500 ) ) ;
#10951 = CARTESIAN_POINT ( 'NONE',  ( 13.13019313627999729, -57.14688517088755759, 4.208364643998075749 ) ) ;
#10952 = CARTESIAN_POINT ( 'NONE',  ( -16.99999999999998579, 2.256146146571129218, 36.00000000000012079 ) ) ;
#10953 = CARTESIAN_POINT ( 'NONE',  ( 30.90276055061299232, -52.52652714576225890, 2.773109545209086590 ) ) ;
#10954 = CARTESIAN_POINT ( 'NONE',  ( 31.72083858694995584, -52.95955415863809179, -2.537984986062459036 ) ) ;
#10955 = CARTESIAN_POINT ( 'NONE',  ( -8.779681704480811533, 2.489320016922789147, 48.36903577193039894 ) ) ;
#10956 = ORIENTED_EDGE ( 'NONE', *, *, #10225, .T. ) ;
#10957 = DIRECTION ( 'NONE',  ( 0.000000000000000000, -1.000000000000000000, 0.000000000000000000 ) ) ;
#10958 = CARTESIAN_POINT ( 'NONE',  ( 33.12582565096496268, -59.20619211347771937, -2.502190571104468741 ) ) ;
#10959 = DIRECTION ( 'NONE',  ( -0.000000000000000000, -0.000000000000000000, -1.000000000000000000 ) ) ;
#10960 = EDGE_CURVE ( 'NONE', #14235, #5016, #5309, .T. ) ;
#10961 = CARTESIAN_POINT ( 'NONE',  ( 9.348584929445154401, -54.69456399997502416, 3.125517714509065570 ) ) ;
#10962 = DIRECTION ( 'NONE',  ( 0.000000000000000000, 1.000000000000000000, -0.000000000000000000 ) ) ;
#10963 = EDGE_CURVE ( 'NONE', #977, #7467, #12165, .T. ) ;
#10964 = DIRECTION ( 'NONE',  ( 0.000000000000000000, 0.000000000000000000, -1.000000000000000000 ) ) ;
#10965 = CARTESIAN_POINT ( 'NONE',  ( -25.21252699837112132, -6.998437922861948657, -48.50000000000011369 ) ) ;
#10966 = VECTOR ( 'NONE', #5623, 1000.000000000000000 ) ;
#10967 = ORIENTED_EDGE ( 'NONE', *, *, #11473, .T. ) ;
#10968 = CARTESIAN_POINT ( 'NONE',  ( 29.07175354616249052, -50.97709764759155604, -4.214141842619275380 ) ) ;
#10969 = VERTEX_POINT ( 'NONE', #10869 ) ;
#10970 = DIRECTION ( 'NONE',  ( 0.000000000000000000, -1.000000000000000000, 0.000000000000000000 ) ) ;
#10971 = FACE_OUTER_BOUND ( 'NONE', #11219, .T. ) ;
#10972 = EDGE_LOOP ( 'NONE', ( #3319, #8076, #8450, #12144 ) ) ;
#10973 = CARTESIAN_POINT ( 'NONE',  ( 54.07385127050791596, 1.678372679529495981, 60.61639468829817190 ) ) ;
#10974 = DIRECTION ( 'NONE',  ( -0.000000000000000000, 1.000000000000000000, 0.000000000000000000 ) ) ;
#10975 = ADVANCED_FACE ( 'NONE', ( #1623 ), #327, .T. ) ;
#10976 = AXIS2_PLACEMENT_3D ( 'NONE', #9409, #6940, #10788 ) ;
#10977 = EDGE_CURVE ( 'NONE', #7233, #3522, #8053, .T. ) ;
#10978 = DIRECTION ( 'NONE',  ( -0.000000000000000000, 0.000000000000000000, 1.000000000000000000 ) ) ;
#10979 = ORIENTED_EDGE ( 'NONE', *, *, #11318, .T. ) ;
#10980 = VERTEX_POINT ( 'NONE', #833 ) ;
#10981 = CARTESIAN_POINT ( 'NONE',  ( -16.99999999999998579, 7.750709400713696517, 38.00000000000012079 ) ) ;
#10982 = LINE ( 'NONE', #440, #10765 ) ;
#10983 = CIRCLE ( 'NONE', #9524, 2.500000000000002220 ) ;
#10984 = ORIENTED_EDGE ( 'NONE', *, *, #7970, .F. ) ;
#10985 = AXIS2_PLACEMENT_3D ( 'NONE', #361, #4824, #9688 ) ;
#10986 = DIRECTION ( 'NONE',  ( 0.000000000000000000, 0.000000000000000000, 1.000000000000000000 ) ) ;
#10987 = VERTEX_POINT ( 'NONE', #5700 ) ;
#10988 =( BOUNDED_SURFACE ( )  B_SPLINE_SURFACE ( 3, 2, ( 
 ( #13390, #5095, #10873 ),
 ( #2565, #14484, #9576 ),
 ( #2710, #1560, #13109 ),
 ( #1481, #7405, #2787 ),
 ( #7482, #8700, #4002 ),
 ( #8493, #10951, #6260 ),
 ( #11939, #3931, #2632 ),
 ( #9800, #9872, #2848 ),
 ( #8627, #12168, #7550 ),
 ( #10796, #8416, #1400 ),
 ( #12247, #176, #6108 ),
 ( #1627, #6327, #14554 ),
 ( #6187, #330, #256 ),
 ( #5024, #11020, #470 ) ),
 .UNSPECIFIED., .F., .F., .F. ) 
 B_SPLINE_SURFACE_WITH_KNOTS ( ( 4, 2, 2, 2, 2, 2, 4 ),
 ( 3, 3 ),
 ( 0.2948322565876035362, 0.2981287057529112827, 0.3014251549182189738, 0.3080180532488344669, 0.3146109515794499600, 0.3179074007447577066, 0.3212038499100654532 ),
 ( 0.000000000000000000, 0.9256633218932661666 ),
 .UNSPECIFIED. ) 
 GEOMETRIC_REPRESENTATION_ITEM ( )  RATIONAL_B_SPLINE_SURFACE ( (
 ( 1.000000000000000000, 0.9979219307738474987, 0.9996910464737041035),
 ( 1.000000000000000000, 0.9979571442240684487, 0.9996962817755321584),
 ( 1.000000000000000000, 0.9979896195972217665, 0.9997011099982531235),
 ( 1.000000000000000000, 0.9980478678147421956, 0.9997097699562453865),
 ( 1.000000000000000000, 0.9980736641738821024, 0.9997136051875368246),
 ( 1.000000000000000000, 0.9981411222205919254, 0.9997236344017447207),
 ( 1.000000000000000000, 0.9981728461536270025, 0.9997283509053414008),
 ( 1.000000000000000000, 0.9982102196781720282, 0.9997339073526689823),
 ( 1.000000000000000000, 0.9982158677593769847, 0.9997347470718578322),
 ( 1.000000000000000000, 0.9982052731646247068, 0.9997331719378983461),
 ( 1.000000000000000000, 0.9981985596398339489, 0.9997321738156357274),
 ( 1.000000000000000000, 0.9981789131846819929, 0.9997292529112105086),
 ( 1.000000000000000000, 0.9981660722458850499, 0.9997273438057426853),
 ( 1.000000000000000000, 0.9981504490785557682, 0.9997250210570212126) ) ) 
 REPRESENTATION_ITEM ( '' )  SURFACE ( )  );
#10989 = CARTESIAN_POINT ( 'NONE',  ( 58.00000000000000711, -2.249290599286311032, 38.00000000000012079 ) ) ;
#10990 = ORIENTED_EDGE ( 'NONE', *, *, #5480, .F. ) ;
#10991 = CARTESIAN_POINT ( 'NONE',  ( 28.75670713205263596, -65.20845675887582615, 3.989712384468892203 ) ) ;
#10992 = AXIS2_PLACEMENT_3D ( 'NONE', #8366, #7046, #7129 ) ;
#10993 = ORIENTED_EDGE ( 'NONE', *, *, #14483, .F. ) ;
#10994 = AXIS2_PLACEMENT_3D ( 'NONE', #14021, #12799, #6942 ) ;
#10995 = DIRECTION ( 'NONE',  ( 1.000000000000000000, 8.673617379884035472E-17, 0.000000000000000000 ) ) ;
#10996 = CARTESIAN_POINT ( 'NONE',  ( 0.000000000000000000, 15.25070940071369563, 139.1143251403882459 ) ) ;
#10997 = EDGE_LOOP ( 'NONE', ( #13335, #6679, #13516, #9218, #13346, #10228, #13724, #8656, #8295, #7010, #1752, #9233, #4243, #11364, #9173, #14001, #10248, #11008, #9308, #1389, #11581, #1245, #1615, #8084 ) ) ;
#10998 = CARTESIAN_POINT ( 'NONE',  ( 27.67989258697571131, -66.53205946168593243, -4.446982897616444497 ) ) ;
#10999 = AXIS2_PLACEMENT_3D ( 'NONE', #9957, #12405, #12179 ) ;
#11000 = ORIENTED_EDGE ( 'NONE', *, *, #12750, .T. ) ;
#11001 = DIRECTION ( 'NONE',  ( -0.000000000000000000, 0.000000000000000000, -1.000000000000000000 ) ) ;
#11002 = LINE ( 'NONE', #14678, #6649 ) ;
#11003 = CARTESIAN_POINT ( 'NONE',  ( -9.271822474830662131, -6.861803161813125662, 47.50000000000012079 ) ) ;
#11004 = AXIS2_PLACEMENT_3D ( 'NONE', #2749, #11266, #11049 ) ;
#11005 = PRODUCT_DEFINITION_FORMATION_WITH_SPECIFIED_SOURCE ( 'ANY', '', #13583, .NOT_KNOWN. ) ;
#11006 = ORIENTED_EDGE ( 'NONE', *, *, #6088, .T. ) ;
#11007 = CARTESIAN_POINT ( 'NONE',  ( 65.83943508202165162, -11.71002111017040193, 72.30872443868064181 ) ) ;
#11008 = ORIENTED_EDGE ( 'NONE', *, *, #157, .F. ) ;
#11009 = VECTOR ( 'NONE', #10718, 1000.000000000000000 ) ;
#11011 = ORIENTED_EDGE ( 'NONE', *, *, #3727, .F. ) ;
#11010 = EDGE_CURVE ( 'NONE', #12204, #7720, #14766, .T. ) ;
#11012 = ORIENTED_EDGE ( 'NONE', *, *, #11188, .F. ) ;
#11013 = CARTESIAN_POINT ( 'NONE',  ( 33.12442989620986822, -59.21224831720011395, -1.832439066039627251 ) ) ;
#11014 = EDGE_CURVE ( 'NONE', #81, #14307, #15002, .T. ) ;
#11015 = APPLICATION_PROTOCOL_DEFINITION ( 'draft international standard', 'automotive_design', 1998, #92 ) ;
#11016 = FACE_OUTER_BOUND ( 'NONE', #2538, .T. ) ;
#11017 = CARTESIAN_POINT ( 'NONE',  ( 13.86173033120691223, -69.39711819508849544, 2.500000000000000000 ) ) ;
#11018 = AXIS2_PLACEMENT_3D ( 'NONE', #4855, #13166, #6173 ) ;
#11019 = FACE_OUTER_BOUND ( 'NONE', #3282, .T. ) ;
#11020 = CARTESIAN_POINT ( 'NONE',  ( 13.88313415068312118, -68.65142943889351557, 4.053691724355805270 ) ) ;
#11021 = CIRCLE ( 'NONE', #10783, 8.500000000000000000 ) ;
#11022 = DIRECTION ( 'NONE',  ( 1.000000000000000000, 0.000000000000000000, -0.000000000000000000 ) ) ;
#11023 = EDGE_CURVE ( 'NONE', #5064, #6181, #12235, .T. ) ;
#11024 = DIRECTION ( 'NONE',  ( 0.000000000000000000, -0.000000000000000000, -1.000000000000000000 ) ) ;
#11025 = EDGE_CURVE ( 'NONE', #9619, #10912, #7564, .T. ) ;
#11026 = CARTESIAN_POINT ( 'NONE',  ( -9.166452524254948386, 2.202000163336201410, 48.23896987259320923 ) ) ;
#11027 = ORIENTED_EDGE ( 'NONE', *, *, #6502, .F. ) ;
#11028 = SURFACE_STYLE_FILL_AREA ( #13336 ) ;
#11029 = CARTESIAN_POINT ( 'NONE',  ( 32.64893181228500652, -58.48798588983608226, -2.754379989675052265 ) ) ;
#11030 = CARTESIAN_POINT ( 'NONE',  ( 43.00000000000000711, 15.25070940071368497, 139.1143251403882459 ) ) ;
#11031 = DIRECTION ( 'NONE',  ( 0.000000000000000000, 1.000000000000000000, 0.000000000000000000 ) ) ;
#11032 = DIRECTION ( 'NONE',  ( 1.000000000000000000, -0.000000000000000000, -0.000000000000000000 ) ) ;
#11033 = PLANE ( 'NONE',  #8386 ) ;
#11034 = CARTESIAN_POINT ( 'NONE',  ( -25.32021674380207799, -6.838035406461215437, -48.10016682092218332 ) ) ;
#11035 = CARTESIAN_POINT ( 'NONE',  ( 32.39917484285220439, 21.75070940071312364, 139.1143251403882459 ) ) ;
#11036 = EDGE_CURVE ( 'NONE', #1083, #12366, #13921, .T. ) ;
#11037 = EDGE_LOOP ( 'NONE', ( #14527, #1368, #8683, #6385, #15079, #2207, #7071, #7114, #5910, #1985 ) ) ;
#11038 = CARTESIAN_POINT ( 'NONE',  ( 65.00000000000001421, -85.24929059928631148, 22.49999999999999289 ) ) ;
#11039 = LINE ( 'NONE', #494, #8420 ) ;
#11040 = EDGE_LOOP ( 'NONE', ( #6997, #2340, #4117, #7914 ) ) ;
#11042 = ORIENTED_EDGE ( 'NONE', *, *, #14497, .F. ) ;
#11041 = DIRECTION ( 'NONE',  ( -0.000000000000000000, 0.000000000000000000, -1.000000000000000000 ) ) ;
#11043 = DIRECTION ( 'NONE',  ( -0.000000000000000000, 0.000000000000000000, 1.000000000000000000 ) ) ;
#11044 = AXIS2_PLACEMENT_3D ( 'NONE', #6329, #5098, #11022 ) ;
#11045 = VECTOR ( 'NONE', #4473, 1000.000000000000000 ) ;
#11046 = CARTESIAN_POINT ( 'NONE',  ( -25.49999999999998934, -2.249290599286303038, 38.00000000000012079 ) ) ;
#11047 = CARTESIAN_POINT ( 'NONE',  ( 93.56770215592470663, 21.75070940071356418, -33.00000000000012790 ) ) ;
#11048 = DIRECTION ( 'NONE',  ( -0.000000000000000000, 1.000000000000000000, -0.000000000000000000 ) ) ;
#11049 = DIRECTION ( 'NONE',  ( 1.000000000000000000, 0.000000000000000000, 0.000000000000000000 ) ) ;
#11050 = CIRCLE ( 'NONE', #1, 0.5000000000000004441 ) ;
#11051 = ORIENTED_EDGE ( 'NONE', *, *, #2924, .F. ) ;
#11052 = DIRECTION ( 'NONE',  ( 1.110223024625156540E-15, -1.000000000000000000, 0.000000000000000000 ) ) ;
#11053 = EDGE_CURVE ( 'NONE', #1708, #4371, #4587, .T. ) ;
#11054 = VERTEX_POINT ( 'NONE', #7772 ) ;
#11055 = DIRECTION ( 'NONE',  ( -0.8746197071345570562, 0.4848096202550665756, 0.000000000000000000 ) ) ;
#11056 = VERTEX_POINT ( 'NONE', #15087 ) ;
#11057 = CARTESIAN_POINT ( 'NONE',  ( 28.31271169503452256, -66.37912134690742505, 3.509717431438163171 ) ) ;
#11058 = ORIENTED_EDGE ( 'NONE', *, *, #12234, .T. ) ;
#11059 = LINE ( 'NONE', #9922, #3599 ) ;
#11060 = DIRECTION ( 'NONE',  ( 1.000000000000000000, 0.000000000000000000, 0.000000000000000000 ) ) ;
#11061 = ORIENTED_EDGE ( 'NONE', *, *, #2144, .F. ) ;
#11062 = VECTOR ( 'NONE', #3441, 1000.000000000000000 ) ;
#11063 = FACE_OUTER_BOUND ( 'NONE', #6295, .T. ) ;
#11064 = EDGE_LOOP ( 'NONE', ( #1924, #5157, #6631, #7960 ) ) ;
#11065 = CARTESIAN_POINT ( 'NONE',  ( 80.00000000000001421, -87.24929059928631148, 35.00000000000000000 ) ) ;
#11066 = DIRECTION ( 'NONE',  ( 0.8656763553492639041, 0.5006040828730973224, 0.000000000000000000 ) ) ;
#11067 = LINE ( 'NONE', #12226, #14577 ) ;
#11068 = ORIENTED_EDGE ( 'NONE', *, *, #5650, .T. ) ;
#11069 = EDGE_CURVE ( 'NONE', #5290, #9032, #13419, .T. ) ;
#11070 = VECTOR ( 'NONE', #562, 1000.000000000000000 ) ;
#11071 = DIRECTION ( 'NONE',  ( 0.2135987722749887463, 0.9769214730379394140, 0.000000000000000000 ) ) ;
#11072 = VERTEX_POINT ( 'NONE', #2070 ) ;
#11073 = ADVANCED_BREP_SHAPE_REPRESENTATION ( '', ( #8947, #6315 ), #417 ) ;
#11074 = ORIENTED_EDGE ( 'NONE', *, *, #4885, .T. ) ;
#11075 = DIRECTION ( 'NONE',  ( -0.000000000000000000, 1.000000000000000000, 0.000000000000000000 ) ) ;
#11076 = TOROIDAL_SURFACE ( 'NONE', #1252, 5.165819364273509073, 0.5000000000000000000 ) ;
#11077 = DIRECTION ( 'NONE',  ( 0.000000000000000000, 0.000000000000000000, 1.000000000000000000 ) ) ;
#11078 = CARTESIAN_POINT ( 'NONE',  ( 59.59091026602544616, -7.053490217115945704, 48.51982618741349285 ) ) ;
#11079 = DIRECTION ( 'NONE',  ( 0.000000000000000000, -1.734723475976817547E-15, -1.000000000000000000 ) ) ;
#11080 = PLANE ( 'NONE',  #4812 ) ;
#11081 = CIRCLE ( 'NONE', #4444, 9.000000000000001776 ) ;
#11082 = ADVANCED_FACE ( 'NONE', ( #13849 ), #7531, .F. ) ;
#11083 = ORIENTED_EDGE ( 'NONE', *, *, #6227, .T. ) ;
#11084 = CARTESIAN_POINT ( 'NONE',  ( -12.14523415828296216, -9.827631355817223024, -48.50000000000012079 ) ) ;
#11085 = CARTESIAN_POINT ( 'NONE',  ( -9.444091399599896519, 2.640528280493846580, 48.24517880332174968 ) ) ;
#11086 = CARTESIAN_POINT ( 'NONE',  ( 13.15370223272280370, -65.65107448351760411, -3.408697305255636412 ) ) ;
#11087 = ORIENTED_EDGE ( 'NONE', *, *, #7402, .T. ) ;
#11088 = CIRCLE ( 'NONE', #12324, 0.7892041907098291675 ) ;
#11089 = AXIS2_PLACEMENT_3D ( 'NONE', #5447, #5605, #3290 ) ;
#11090 = AXIS2_PLACEMENT_3D ( 'NONE', #2108, #1106, #7038 ) ;
#11091 = CARTESIAN_POINT ( 'NONE',  ( -9.037775043065352065, 2.932694901963889489, 58.00000000000012079 ) ) ;
#11092 = EDGE_CURVE ( 'NONE', #931, #879, #885, .T. ) ;
#11093 = ORIENTED_EDGE ( 'NONE', *, *, #2072, .F. ) ;
#11094 = LINE ( 'NONE', #480, #8632 ) ;
#11095 = CARTESIAN_POINT ( 'NONE',  ( 33.52235686305655804, -57.48563641131178770, -1.816685854991397564 ) ) ;
#11096 = DIRECTION ( 'NONE',  ( 1.000000000000000000, 0.000000000000000000, 0.000000000000000000 ) ) ;
#11097 = DIRECTION ( 'NONE',  ( -0.000000000000000000, 0.000000000000000000, -1.000000000000000000 ) ) ;
#11098 = ORIENTED_EDGE ( 'NONE', *, *, #12071, .T. ) ;
#11099 = EDGE_CURVE ( 'NONE', #1157, #6894, #13196, .T. ) ;
#11100 = ADVANCED_FACE ( 'NONE', ( #10083 ), #4009, .T. ) ;
#11101 = FACE_OUTER_BOUND ( 'NONE', #8081, .T. ) ;
#11102 = EDGE_CURVE ( 'NONE', #8405, #11391, #1393, .T. ) ;
#11103=STYLED_ITEM('',(#15244),#14171);
#11104 = DIRECTION ( 'NONE',  ( 0.5454721580263448555, -0.8381289428352193260, -0.000000000000000000 ) ) ;
#11105 = AXIS2_PLACEMENT_3D ( 'NONE', #7995, #1065, #5619 ) ;
#11106 = AXIS2_PLACEMENT_3D ( 'NONE', #6407, #11104, #8475 ) ;
#11107 = CARTESIAN_POINT ( 'NONE',  ( -8.958610760419841057, 1.823307968896474840, -58.00000000000012079 ) ) ;
#11108 = ADVANCED_FACE ( 'NONE', ( #3225 ), #7929, .F. ) ;
#11109 = CARTESIAN_POINT ( 'NONE',  ( -25.27051402993791029, -6.915952606384455414, -48.19241902544784750 ) ) ;
#11110 = EDGE_LOOP ( 'NONE', ( #6400, #12422, #220, #2821 ) ) ;
#11111 = FACE_OUTER_BOUND ( 'NONE', #1856, .T. ) ;
#11112=STYLED_ITEM('',(#15272),#14540);
#11113 = VECTOR ( 'NONE', #5539, 1000.000000000000000 ) ;
#11114 = ORIENTED_EDGE ( 'NONE', *, *, #3210, .T. ) ;
#11115 = DIRECTION ( 'NONE',  ( 0.000000000000000000, 0.000000000000000000, -1.000000000000000000 ) ) ;
#11116 = PLANE ( 'NONE',  #7666 ) ;
#11117 = CIRCLE ( 'NONE', #14071, 0.5000000000000004441 ) ;
#11118 = ORIENTED_EDGE ( 'NONE', *, *, #14553, .T. ) ;
#11119 = DIRECTION ( 'NONE',  ( 0.8746197071345569451, -0.4848096202550666312, 0.000000000000000000 ) ) ;
#11120 = LINE ( 'NONE', #1808, #7786 ) ;
#11121 = EDGE_CURVE ( 'NONE', #6007, #9917, #11611, .T. ) ;
#11122 = DIRECTION ( 'NONE',  ( 0.000000000000000000, 1.000000000000000000, -0.000000000000000000 ) ) ;
#11123 = VECTOR ( 'NONE', #8355, 1000.000000000000000 ) ;
#11124 = CARTESIAN_POINT ( 'NONE',  ( 9.664729663202141552, -53.19870790407432537, 3.318692829847595505 ) ) ;
#11125 = CARTESIAN_POINT ( 'NONE',  ( 100.0000000000000284, 0.000000000000000000, 33.00000000000012790 ) ) ;
#11126 = LINE ( 'NONE', #1593, #5601 ) ;
#11127 = VECTOR ( 'NONE', #7554, 1000.000000000000000 ) ;
#11128 = VERTEX_POINT ( 'NONE', #12862 ) ;
#11129 = DIRECTION ( 'NONE',  ( 1.000000000000000000, 0.000000000000000000, 0.000000000000000000 ) ) ;
#11130 = ORIENTED_EDGE ( 'NONE', *, *, #4617, .F. ) ;
#11131 = FACE_OUTER_BOUND ( 'NONE', #1225, .T. ) ;
#11132 = VERTEX_POINT ( 'NONE', #8391 ) ;
#11133 = FACE_OUTER_BOUND ( 'NONE', #2530, .T. ) ;
#11134 = B_SPLINE_CURVE_WITH_KNOTS ( 'NONE', 3,
 ( #3412, #3491, #2334, #10573, #31, #9421, #8269, #9813, #4163, #6201 ),
 .UNSPECIFIED., .F., .F.,
 ( 4, 2, 2, 2, 4 ),
 ( 0.000000000000000000, 0.0003835113287520874100, 0.0007670226575041748200, 0.001150533986256262230, 0.001534045315008349640 ),
 .UNSPECIFIED. ) ;
#11135 = B_SPLINE_CURVE_WITH_KNOTS ( 'NONE', 3,
 ( #11762, #2377, #10840, #10540, #11911, #1371, #6075, #12857, #301, #9703, #7076, #3457, #12209, #12285 ),
 .UNSPECIFIED., .F., .F.,
 ( 4, 2, 2, 2, 2, 2, 4 ),
 ( 1.788112030672749005E-18, 0.002516897397286753553, 0.003775346095930122957, 0.005033794794573492361, 0.006292243493216862632, 0.007550692191860232903, 0.01006758958914701074 ),
 .UNSPECIFIED. ) ;
#11136 = CARTESIAN_POINT ( 'NONE',  ( 64.90552635791956959, 22.43695620243006772, 84.20452624982236500 ) ) ;
#11137 = EDGE_CURVE ( 'NONE', #11210, #6839, #9552, .T. ) ;
#11138 = AXIS2_PLACEMENT_3D ( 'NONE', #14735, #8889, #723 ) ;
#11139 = LINE ( 'NONE', #6373, #13677 ) ;
#11140 = LINE ( 'NONE', #6241, #2802 ) ;
#11141 = VERTEX_POINT ( 'NONE', #2872 ) ;
#11142 = VECTOR ( 'NONE', #12001, 1000.000000000000000 ) ;
#11143 = DIRECTION ( 'NONE',  ( 0.000000000000000000, -1.000000000000000000, -2.081668171172168119E-15 ) ) ;
#11144 = ORIENTED_EDGE ( 'NONE', *, *, #14180, .F. ) ;
#11145 = EDGE_CURVE ( 'NONE', #6102, #587, #11841, .T. ) ;
#11146 = EDGE_CURVE ( 'NONE', #4250, #14153, #1376, .T. ) ;
#11147 = LINE ( 'NONE', #7609, #423 ) ;
#11148 = CARTESIAN_POINT ( 'NONE',  ( 12.02094163398139237, -52.24929059928630437, -4.175384597093462880 ) ) ;
#11149 = DIRECTION ( 'NONE',  ( -0.000000000000000000, 1.000000000000000000, 1.445602896647339163E-16 ) ) ;
#11150 = LINE ( 'NONE', #7763, #4759 ) ;
#11151 = EDGE_LOOP ( 'NONE', ( #3396, #2131, #24, #12737 ) ) ;
#11152 = CARTESIAN_POINT ( 'NONE',  ( 112.9262740340969060, 21.75070940071369918, -13.14990448602693007 ) ) ;
#11153 = ORIENTED_EDGE ( 'NONE', *, *, #13676, .T. ) ;
#11154 = ORIENTED_EDGE ( 'NONE', *, *, #11102, .T. ) ;
#11155 = VERTEX_POINT ( 'NONE', #6081 ) ;
#11156 = DIRECTION ( 'NONE',  ( 0.000000000000000000, -0.000000000000000000, 1.000000000000000000 ) ) ;
#11157 = DIRECTION ( 'NONE',  ( 0.000000000000000000, 0.000000000000000000, 1.000000000000000000 ) ) ;
#11158 = CARTESIAN_POINT ( 'NONE',  ( 13.86173033120691223, -69.39711819508849544, 2.500000000000000000 ) ) ;
#11159 = ADVANCED_FACE ( 'NONE', ( #3540 ), #1071, .F. ) ;
#11160 = DIRECTION ( 'NONE',  ( 0.000000000000000000, 1.000000000000000000, -0.000000000000000000 ) ) ;
#11161 = EDGE_CURVE ( 'NONE', #5809, #7882, #9009, .T. ) ;
#11162 = ORIENTED_EDGE ( 'NONE', *, *, #740, .F. ) ;
#11163 = CARTESIAN_POINT ( 'NONE',  ( 65.26950693702184481, -11.12283941681556954, 72.18019809873047166 ) ) ;
#11164 = FACE_OUTER_BOUND ( 'NONE', #13765, .T. ) ;
#11165 = CARTESIAN_POINT ( 'NONE',  ( -9.041069614211208361, 1.954516911250973932, 47.50000000000011369 ) ) ;
#11166 = DIRECTION ( 'NONE',  ( 8.673617379884035472E-17, -1.000000000000000000, 0.000000000000000000 ) ) ;
#11167 = VERTEX_POINT ( 'NONE', #14236 ) ;
#11168 = FACE_OUTER_BOUND ( 'NONE', #4120, .T. ) ;
#11169 = CARTESIAN_POINT ( 'NONE',  ( -9.354272893020521451, 2.499447352334152050, 47.88483805351501132 ) ) ;
#11170 = EDGE_LOOP ( 'NONE', ( #12926, #3150, #12402, #12053 ) ) ;
#11171 = DIRECTION ( 'NONE',  ( 0.000000000000000000, 0.000000000000000000, -1.000000000000000000 ) ) ;
#11172 = CARTESIAN_POINT ( 'NONE',  ( 8.127555659019208179, -57.16650977415540069, -1.814547216390245632 ) ) ;
#11173 = LINE ( 'NONE', #1855, #910 ) ;
#11174 = ORIENTED_EDGE ( 'NONE', *, *, #5087, .T. ) ;
#11175 = CARTESIAN_POINT ( 'NONE',  ( 17.09549820959326638, -82.24929059928629727, 1.347403282660979640 ) ) ;
#11176 = EDGE_CURVE ( 'NONE', #166, #1026, #15156, .T. ) ;
#11177 = CARTESIAN_POINT ( 'NONE',  ( 53.11142512232702018, -3.558169932106523881, 62.84860122826521689 ) ) ;
#11178 = DIRECTION ( 'NONE',  ( 0.000000000000000000, 0.000000000000000000, -1.000000000000000000 ) ) ;
#11179 = CARTESIAN_POINT ( 'NONE',  ( 55.09646579789918519, -6.394265699299607419, 62.84860122826521689 ) ) ;
#11180 = ORIENTED_EDGE ( 'NONE', *, *, #9195, .F. ) ;
#11181 = CARTESIAN_POINT ( 'NONE',  ( 23.59140218557817192, -57.03285117764829693, -6.445925775548339232 ) ) ;
#11182 = ORIENTED_EDGE ( 'NONE', *, *, #2930, .T. ) ;
#11183 = CARTESIAN_POINT ( 'NONE',  ( 80.00000000000001421, -87.24929059928631148, -35.00000000000000000 ) ) ;
#11184 = CARTESIAN_POINT ( 'NONE',  ( -33.07225206673494711, -1.856991049495498425, -48.00000000000012079 ) ) ;
#11185 = VERTEX_POINT ( 'NONE', #12780 ) ;
#11186 = FACE_BOUND ( 'NONE', #13532, .T. ) ;
#11187 = DIRECTION ( 'NONE',  ( 0.8420378618367723167, 0.5394184268574414576, -0.000000000000000000 ) ) ;
#11188 = EDGE_CURVE ( 'NONE', #4627, #1474, #9468, .T. ) ;
#11189 = EDGE_CURVE ( 'NONE', #9615, #556, #10232, .T. ) ;
#11190 = CLOSED_SHELL ( 'NONE', ( #7868, #3008, #654, #8166, #14682, #1387, #9657, #7487, #14856, #3528, #2951, #123, #12507, #15101, #2942, #9854, #5171, #10054 ) ) ;
#11191 = CARTESIAN_POINT ( 'NONE',  ( 12.92924986285039957, -63.81378734511389439, 4.043274055231490749 ) ) ;
#11192 = AXIS2_PLACEMENT_3D ( 'NONE', #10871, #14409, #4868 ) ;
#11193 = DIRECTION ( 'NONE',  ( -1.000000000000000000, 0.000000000000000000, 0.000000000000000000 ) ) ;
#11194 = CARTESIAN_POINT ( 'NONE',  ( 58.00000000000000711, -2.249290599286307479, 33.00000000000012790 ) ) ;
#11195 = CARTESIAN_POINT ( 'NONE',  ( -5.290523468902621929, 4.522075770548486418, 48.00000000000012079 ) ) ;
#11196 = EDGE_CURVE ( 'NONE', #358, #1788, #11688, .T. ) ;
#11197 = ORIENTED_EDGE ( 'NONE', *, *, #15171, .F. ) ;
#11198 = EDGE_CURVE ( 'NONE', #8798, #1834, #8241, .T. ) ;
#11199 = DIRECTION ( 'NONE',  ( 0.000000000000000000, -1.000000000000000000, 0.000000000000000000 ) ) ;
#11200 = ORIENTED_EDGE ( 'NONE', *, *, #1226, .F. ) ;
#11201 = CARTESIAN_POINT ( 'NONE',  ( -23.19801677984724364, 4.285555568094122414, 47.93908580834070676 ) ) ;
#11202 = EDGE_LOOP ( 'NONE', ( #2508, #13192, #4011, #666 ) ) ;
#11203 = CARTESIAN_POINT ( 'NONE',  ( 58.00000000000000711, -2.249290599286307479, 38.00000000000012079 ) ) ;
#11204 = VECTOR ( 'NONE', #3286, 1000.000000000000000 ) ;
#11205 = CARTESIAN_POINT ( 'NONE',  ( 69.46451213741848107, -2.308034861962666717, 72.93576380291801797 ) ) ;
#11206 = CARTESIAN_POINT ( 'NONE',  ( -25.99999999999998934, -2.249290599286303927, -47.50000000000012079 ) ) ;
#11207 = DIRECTION ( 'NONE',  ( 0.000000000000000000, 1.000000000000000000, -0.000000000000000000 ) ) ;
#11208 = ORIENTED_EDGE ( 'NONE', *, *, #3310, .F. ) ;
#11209 = DIRECTION ( 'NONE',  ( 1.000000000000000000, 0.000000000000000000, 0.000000000000000000 ) ) ;
#11210 = VERTEX_POINT ( 'NONE', #9625 ) ;
#11211 = VECTOR ( 'NONE', #376, 1000.000000000000000 ) ;
#11212 = AXIS2_PLACEMENT_3D ( 'NONE', #10597, #13287, #3812 ) ;
#11213 = CARTESIAN_POINT ( 'NONE',  ( 11.79320013990377802, -53.28555914635324342, -4.056187502120401689 ) ) ;
#11214 = LINE ( 'NONE', #2062, #332 ) ;
#11215 = CARTESIAN_POINT ( 'NONE',  ( 61.18622467607353599, 2.299242679852274929, 48.51982618741349285 ) ) ;
#11216 = ORIENTED_EDGE ( 'NONE', *, *, #11389, .T. ) ;
#11217 = CARTESIAN_POINT ( 'NONE',  ( -16.99999999999998579, 2.256146146571129218, 36.00000000000012079 ) ) ;
#11218 = VECTOR ( 'NONE', #13227, 1000.000000000000000 ) ;
#11219 = EDGE_LOOP ( 'NONE', ( #2921, #6819, #6527, #11308 ) ) ;
#11220 = VERTEX_POINT ( 'NONE', #1140 ) ;
#11221 = ORIENTED_EDGE ( 'NONE', *, *, #9676, .F. ) ;
#11222 = EDGE_CURVE ( 'NONE', #9708, #3099, #6013, .T. ) ;
#11224 = AXIS2_PLACEMENT_3D ( 'NONE', #12156, #7533, #3769 ) ;
#11223 =( NAMED_UNIT ( * ) PLANE_ANGLE_UNIT ( ) SI_UNIT ( $, .RADIAN. ) );
#11225 = VECTOR ( 'NONE', #10661, 1000.000000000000114 ) ;
#11226 = DIRECTION ( 'NONE',  ( -0.01745240642731254316, 0.9998476951565652415, 0.000000000000000000 ) ) ;
#11227 = CARTESIAN_POINT ( 'NONE',  ( 71.76344687472122530, -15.59526412071138957, 73.07464432123545350 ) ) ;
#11228 = EDGE_CURVE ( 'NONE', #8509, #7521, #5862, .T. ) ;
#11229 = CARTESIAN_POINT ( 'NONE',  ( 62.80738265182633739, -4.914066317053380040, 87.40005259842790508 ) ) ;
#11230 = EDGE_LOOP ( 'NONE', ( #3073, #14609, #3586, #3162 ) ) ;
#11231 = AXIS2_PLACEMENT_3D ( 'NONE', #14974, #11500, #4422 ) ;
#11232 = CARTESIAN_POINT ( 'NONE',  ( 65.81539560090801899, -11.71715063578952964, 72.32462332011485273 ) ) ;
#11233 = CARTESIAN_POINT ( 'NONE',  ( 69.30413741146281836, -4.165477212746960589, 77.19766410831375936 ) ) ;
#11234 = VECTOR ( 'NONE', #8247, 1000.000000000000000 ) ;
#11235 = CARTESIAN_POINT ( 'NONE',  ( 66.38598137497019991, -11.47113225237460910, 76.19766410831374515 ) ) ;
#11236 = FACE_OUTER_BOUND ( 'NONE', #14238, .T. ) ;
#11237 = ORIENTED_EDGE ( 'NONE', *, *, #4521, .F. ) ;
#11238 = VECTOR ( 'NONE', #1397, 1000.000000000000000 ) ;
#11239 = CARTESIAN_POINT ( 'NONE',  ( 108.0866310645538562, 21.75070940071366365, 13.14990448602693007 ) ) ;
#11240 = EDGE_CURVE ( 'NONE', #10817, #10346, #7239, .T. ) ;
#11241 = VERTEX_POINT ( 'NONE', #3761 ) ;
#11242 = EDGE_CURVE ( 'NONE', #13978, #10292, #14652, .T. ) ;
#11243 = CARTESIAN_POINT ( 'NONE',  ( 28.24952126317575818, -64.89111109908230901, -4.244693487287873879 ) ) ;
#11244 = DIRECTION ( 'NONE',  ( -1.000000000000000000, 0.000000000000000000, -0.000000000000000000 ) ) ;
#11245 = AXIS2_PLACEMENT_3D ( 'NONE', #2081, #3395, #11699 ) ;
#11246 = DIRECTION ( 'NONE',  ( 0.000000000000000000, 1.000000000000000000, 0.000000000000000000 ) ) ;
#11247 = VECTOR ( 'NONE', #10336, 1000.000000000000000 ) ;
#11248 = CARTESIAN_POINT ( 'NONE',  ( 9.657759076947806776, -54.31552982368702942, 3.256647958671365917 ) ) ;
#11249 = DIRECTION ( 'NONE',  ( -0.000000000000000000, -0.000000000000000000, 1.000000000000000000 ) ) ;
#11250 = DIRECTION ( 'NONE',  ( 0.000000000000000000, 0.000000000000000000, 1.000000000000000000 ) ) ;
#11251 = CARTESIAN_POINT ( 'NONE',  ( -24.85140262670387301, -6.666068128078234345, -48.18452149279842445 ) ) ;
#11252 = ORIENTED_EDGE ( 'NONE', *, *, #7639, .T. ) ;
#11253 = EDGE_CURVE ( 'NONE', #3805, #2373, #10929, .T. ) ;
#11254 = DIRECTION ( 'NONE',  ( 1.000000000000000000, 0.000000000000000000, -0.000000000000000000 ) ) ;
#11255 = ORIENTED_EDGE ( 'NONE', *, *, #6358, .T. ) ;
#11256 = CARTESIAN_POINT ( 'NONE',  ( 58.00000000000000711, -2.249290599286309256, 87.40005259842790508 ) ) ;
#11257 = DIRECTION ( 'NONE',  ( -1.000000000000000000, 0.000000000000000000, 0.000000000000000000 ) ) ;
#11258 = VERTEX_POINT ( 'NONE', #2608 ) ;
#11259 = LINE ( 'NONE', #12743, #540 ) ;
#11260 = CARTESIAN_POINT ( 'NONE',  ( 13.86173033120691223, -69.39711819508849544, -3.619682905202625811 ) ) ;
#11261 = ORIENTED_EDGE ( 'NONE', *, *, #2174, .T. ) ;
#11262 = CARTESIAN_POINT ( 'NONE',  ( 70.46453521882888538, -2.298370886119716960, 73.19766410831374515 ) ) ;
#11263 = LINE ( 'NONE', #9906, #3641 ) ;
#11264 = CARTESIAN_POINT ( 'NONE',  ( 58.00000000000000711, -2.249290599286309256, 81.40005259842790508 ) ) ;
#11265 = CARTESIAN_POINT ( 'NONE',  ( -16.99999999999998579, -12.24929059928630437, 38.00000000000012079 ) ) ;
#11266 = DIRECTION ( 'NONE',  ( 0.000000000000000000, 0.000000000000000000, 1.000000000000000000 ) ) ;
#11267 = ORIENTED_EDGE ( 'NONE', *, *, #9044, .T. ) ;
#11268 = DIRECTION ( 'NONE',  ( 0.000000000000000000, 1.000000000000000000, 0.000000000000000000 ) ) ;
#11269 = ORIENTED_EDGE ( 'NONE', *, *, #7518, .F. ) ;
#11270 = CARTESIAN_POINT ( 'NONE',  ( -16.99999999999998579, -2.249290599286303927, -57.50000000000012079 ) ) ;
#11271 = AXIS2_PLACEMENT_3D ( 'NONE', #6547, #14942, #11244 ) ;
#11272 = ORIENTED_EDGE ( 'NONE', *, *, #1068, .T. ) ;
#11273 = CARTESIAN_POINT ( 'NONE',  ( 27.86203511185233594, -69.48056866272028742, 4.214447830835810649 ) ) ;
#11274 = CARTESIAN_POINT ( 'NONE',  ( 52.50499674461036648, -3.053107681157296582, 48.51982618741349285 ) ) ;
#11275 = CARTESIAN_POINT ( 'NONE',  ( -16.99999999999998579, -6.754727345143736628, 38.00000000000012079 ) ) ;
#11276 = CARTESIAN_POINT ( 'NONE',  ( 40.00000000000002132, -74.24929059928642516, 32.99999999999999289 ) ) ;
#11277 = VERTEX_POINT ( 'NONE', #7602 ) ;
#11278 = ADVANCED_FACE ( 'NONE', ( #12216 ), #5142, .T. ) ;
#11279 = EDGE_CURVE ( 'NONE', #13060, #3355, #10734, .T. ) ;
#11280 = CARTESIAN_POINT ( 'NONE',  ( 27.86188286885952081, -69.45278782524461292, -3.616934341765170036 ) ) ;
#11281 = VERTEX_POINT ( 'NONE', #1605 ) ;
#11282 = B_SPLINE_CURVE_WITH_KNOTS ( 'NONE', 3,
 ( #3331, #11478, #10338, #7107 ),
 .UNSPECIFIED., .F., .F.,
 ( 4, 4 ),
 ( 0.000000000000000000, 0.001771361151111836311 ),
 .UNSPECIFIED. ) ;
#11283 = VECTOR ( 'NONE', #3471, 1000.000000000000000 ) ;
#11284 = TOROIDAL_SURFACE ( 'NONE', #7132, 9.500000000000001776, 0.5000000000000000000 ) ;
#11285 = DIRECTION ( 'NONE',  ( 0.8656763553493062036, 0.5006040828730242698, 0.000000000000000000 ) ) ;
#11286 = CARTESIAN_POINT ( 'NONE',  ( 12.44985739169131556, -58.32476007869853873, 2.500000000000000000 ) ) ;
#11287 = CARTESIAN_POINT ( 'NONE',  ( -12.14523415828296216, -9.827631355817223024, -57.50000000000012079 ) ) ;
#11288 = DIRECTION ( 'NONE',  ( 0.4848096202550660205, 0.8746197071345573892, 0.000000000000000000 ) ) ;
#11289 = EDGE_CURVE ( 'NONE', #10251, #12406, #11990, .T. ) ;
#11290 = ORIENTED_EDGE ( 'NONE', *, *, #14094, .F. ) ;
#11291 = CARTESIAN_POINT ( 'NONE',  ( -12.99999999999998757, -67.96969602390581144, 33.00000000000001421 ) ) ;
#11292 = VERTEX_POINT ( 'NONE', #8537 ) ;
#11293 = CARTESIAN_POINT ( 'NONE',  ( -5.040221427466104132, 4.089237592873841365, 48.50000000000012079 ) ) ;
#11294 = ORIENTED_EDGE ( 'NONE', *, *, #12710, .T. ) ;
#11295 = ORIENTED_EDGE ( 'NONE', *, *, #9422, .F. ) ;
#11296 = CARTESIAN_POINT ( 'NONE',  ( -8.499999999999987566, -2.249290599286303927, -38.50000000000012790 ) ) ;
#11297 = AXIS2_PLACEMENT_3D ( 'NONE', #7459, #3684, #11837 ) ;
#11298 = CARTESIAN_POINT ( 'NONE',  ( -16.99999999999998579, -2.249290599286303927, 33.00000000000012790 ) ) ;
#11299 = CARTESIAN_POINT ( 'NONE',  ( -22.42998452855183444, 4.960558937058127782, -48.26605223428308733 ) ) ;
#11300 = CARTESIAN_POINT ( 'NONE',  ( 27.55953187330915810, 23.25070940071368852, 139.1143251403882459 ) ) ;
#11301 = EDGE_LOOP ( 'NONE', ( #2826, #11877 ) ) ;
#11302 = CARTESIAN_POINT ( 'NONE',  ( -8.787473001628837821, 2.499856724289235554, -48.36782213136056896 ) ) ;
#11303 = CARTESIAN_POINT ( 'NONE',  ( 70.25075942771931636, -4.321398257530866260, 76.19766410831374515 ) ) ;
#11304 = CARTESIAN_POINT ( 'NONE',  ( 69.46454297106443221, -2.294433322023680333, 75.32995078675688205 ) ) ;
#11305 = ADVANCED_FACE ( 'NONE', ( #7525 ), #13156, .F. ) ;
#11306 = CARTESIAN_POINT ( 'NONE',  ( 20.86173033120691045, -72.24929059928631148, 0.000000000000000000 ) ) ;
#11307 = CARTESIAN_POINT ( 'NONE',  ( 11.46205536272672454, -61.79747627231519402, -3.500139319476019750 ) ) ;
#11308 = ORIENTED_EDGE ( 'NONE', *, *, #2672, .F. ) ;
#11309 = CARTESIAN_POINT ( 'NONE',  ( 69.97972560191894331, -3.172990595108510004, 73.12858342702070047 ) ) ;
#11310 = CARTESIAN_POINT ( 'NONE',  ( 0.000000000000000000, 21.75070940071319114, 139.1143251403882459 ) ) ;
#11311 = VERTEX_POINT ( 'NONE', #14528 ) ;
#11312 = DIRECTION ( 'NONE',  ( -0.8656763553492640151, -0.5006040828730974335, -0.000000000000000000 ) ) ;
#11313 = CARTESIAN_POINT ( 'NONE',  ( 58.14816640453862107, 2.809303687574978614, 48.51982618741349285 ) ) ;
#11314 = LINE ( 'NONE', #8100, #8893 ) ;
#11315 = ORIENTED_EDGE ( 'NONE', *, *, #13841, .F. ) ;
#11316 = DIRECTION ( 'NONE',  ( -1.000000000000000000, 0.000000000000000000, 0.000000000000000000 ) ) ;
#11317 = AXIS2_PLACEMENT_3D ( 'NONE', #7277, #3667, #11966 ) ;
#11318 = EDGE_CURVE ( 'NONE', #7093, #1111, #3978, .T. ) ;
#11319 = CYLINDRICAL_SURFACE ( 'NONE', #2691, 7.000000000000000000 ) ;
#11320 = EDGE_CURVE ( 'NONE', #11520, #2756, #14464, .T. ) ;
#11321 = DIRECTION ( 'NONE',  ( 0.1334096321106371386, -0.9910609820087281641, 0.000000000000000000 ) ) ;
#11322 = FACE_OUTER_BOUND ( 'NONE', #10134, .T. ) ;
#11323 = CIRCLE ( 'NONE', #11090, 0.5000000000000004441 ) ;
#11324 = ORIENTED_EDGE ( 'NONE', *, *, #11557, .F. ) ;
#11325 = ORIENTED_EDGE ( 'NONE', *, *, #9488, .T. ) ;
#11326 = DIRECTION ( 'NONE',  ( 0.000000000000000000, -0.000000000000000000, 1.000000000000000000 ) ) ;
#11327 = VERTEX_POINT ( 'NONE', #5217 ) ;
#11328 = DIRECTION ( 'NONE',  ( 0.000000000000000000, 0.000000000000000000, 1.000000000000000000 ) ) ;
#11329 = CARTESIAN_POINT ( 'NONE',  ( -65.00000000000001421, -85.24929059928631148, 19.99999999999999645 ) ) ;
#11330 = ORIENTED_EDGE ( 'NONE', *, *, #3854, .T. ) ;
#11331 = ORIENTED_EDGE ( 'NONE', *, *, #1119, .F. ) ;
#11332 = VECTOR ( 'NONE', #14724, 1000.000000000000000 ) ;
#11333 = LINE ( 'NONE', #5510, #2276 ) ;
#11334 = DIRECTION ( 'NONE',  ( 0.000000000000000000, 0.000000000000000000, 1.000000000000000000 ) ) ;
#11335 = AXIS2_PLACEMENT_3D ( 'NONE', #12937, #6084, #14009 ) ;
#11336 = CIRCLE ( 'NONE', #4724, 0.7892041907098306108 ) ;
#11337 = CARTESIAN_POINT ( 'NONE',  ( 12.61580082134570269, -64.50532980541186134, 3.862852061923984337 ) ) ;
#11338 = EDGE_CURVE ( 'NONE', #11898, #619, #6161, .T. ) ;
#11339 = EDGE_CURVE ( 'NONE', #3036, #3165, #8524, .T. ) ;
#11340 = CARTESIAN_POINT ( 'NONE',  ( -8.779641963837230279, 13.70511383897430058, -48.00000000000012079 ) ) ;
#11341 = CARTESIAN_POINT ( 'NONE',  ( 32.31055461597316025, -59.69871785856275181, 2.790504257380250319 ) ) ;
#11342 = FACE_OUTER_BOUND ( 'NONE', #14472, .T. ) ;
#11343 = DIRECTION ( 'NONE',  ( -0.000000000000000000, 1.000000000000000000, 1.445602896647339163E-16 ) ) ;
#11344 = VECTOR ( 'NONE', #9180, 1000.000000000000000 ) ;
#11345 = FACE_OUTER_BOUND ( 'NONE', #378, .T. ) ;
#11346 = EDGE_LOOP ( 'NONE', ( #1722, #15106, #11595, #10255 ) ) ;
#11347 = CARTESIAN_POINT ( 'NONE',  ( 17.40655560129473756, -73.00063092935795339, -6.088059227058379541 ) ) ;
#11348 = VECTOR ( 'NONE', #84, 1000.000000000000000 ) ;
#11349 = VERTEX_POINT ( 'NONE', #2829 ) ;
#11350 = VERTEX_POINT ( 'NONE', #7381 ) ;
#11351 = CARTESIAN_POINT ( 'NONE',  ( 28.21768499689855503, -66.70046270226332297, 4.174231074483972570 ) ) ;
#11352 = DIRECTION ( 'NONE',  ( 0.000000000000000000, 0.000000000000000000, 1.000000000000000000 ) ) ;
#11353 = AXIS2_PLACEMENT_3D ( 'NONE', #11296, #11075, #4293 ) ;
#11354 = DIRECTION ( 'NONE',  ( -1.000000000000000000, 0.000000000000000000, 0.000000000000000000 ) ) ;
#11355 = DIRECTION ( 'NONE',  ( 0.000000000000000000, -1.000000000000000000, 0.000000000000000000 ) ) ;
#11356 = DIRECTION ( 'NONE',  ( 1.000000000000000000, 0.000000000000000000, 0.000000000000000000 ) ) ;
#11357 = ORIENTED_EDGE ( 'NONE', *, *, #1790, .T. ) ;
#11358 = AXIS2_PLACEMENT_3D ( 'NONE', #6284, #6062, #10753 ) ;
#11359 = LINE ( 'NONE', #10217, #2204 ) ;
#11360 = CARTESIAN_POINT ( 'NONE',  ( 8.844813971085542903, -54.08909618700739230, -2.984935890591794205 ) ) ;
#11361 = CARTESIAN_POINT ( 'NONE',  ( -20.99999999999998579, -2.249290599286302594, 33.00000000000012790 ) ) ;
#11362 = ADVANCED_FACE ( 'NONE', ( #5000 ), #9706, .F. ) ;
#11363 = CARTESIAN_POINT ( 'NONE',  ( -9.334567670938534789, -7.621465217813490511, 48.02064173568530236 ) ) ;
#11364 = ORIENTED_EDGE ( 'NONE', *, *, #6572, .F. ) ;
#11365 = ORIENTED_EDGE ( 'NONE', *, *, #9818, .T. ) ;
#11366 = DIRECTION ( 'NONE',  ( -0.000000000000000000, -0.000000000000000000, -1.000000000000000000 ) ) ;
#11367 = EDGE_CURVE ( 'NONE', #6567, #11241, #3832, .T. ) ;
#11368 = VERTEX_POINT ( 'NONE', #13237 ) ;
#11369 = CARTESIAN_POINT ( 'NONE',  ( -1.197457146693678531, -2.220571218158920779, -48.50000000000012079 ) ) ;
#11370 = ORIENTED_EDGE ( 'NONE', *, *, #12920, .T. ) ;
#11371 = ADVANCED_FACE ( 'NONE', ( #6443 ), #13301, .F. ) ;
#11372 = CIRCLE ( 'NONE', #9907, 31.00000000000000000 ) ;
#11373 = ORIENTED_EDGE ( 'NONE', *, *, #3193, .T. ) ;
#11374 = VECTOR ( 'NONE', #1310, 1000.000000000000114 ) ;
#11375 = CARTESIAN_POINT ( 'NONE',  ( -16.99999999999998579, -2.249290599286303927, -47.50000000000012079 ) ) ;
#11376 = CARTESIAN_POINT ( 'NONE',  ( -3.999999999999976019, -72.24929059928631148, 33.00000000000000000 ) ) ;
#11377 = EDGE_CURVE ( 'NONE', #4665, #13009, #11139, .T. ) ;
#11378 = EDGE_CURVE ( 'NONE', #12689, #538, #11059, .T. ) ;
#11379 = PLANE ( 'NONE',  #4311 ) ;
#11380 = LINE ( 'NONE', #14569, #2003 ) ;
#11381 = ORIENTED_EDGE ( 'NONE', *, *, #11664, .F. ) ;
#11382 = PLANE ( 'NONE',  #2423 ) ;
#11383 = FACE_OUTER_BOUND ( 'NONE', #4073, .T. ) ;
#11384 = DIRECTION ( 'NONE',  ( 0.3020115420618285085, -0.1674077314120178406, 0.9384901064608609511 ) ) ;
#11385 = CARTESIAN_POINT ( 'NONE',  ( 32.10796813252333948, -61.48517313025205766, 2.719255632294420799 ) ) ;
#11386 = VECTOR ( 'NONE', #2054, 1000.000000000000000 ) ;
#11387 = ORIENTED_EDGE ( 'NONE', *, *, #11424, .T. ) ;
#11388 = ADVANCED_FACE ( 'NONE', ( #4047 ), #5293, .F. ) ;
#11389 = EDGE_CURVE ( 'NONE', #9348, #10924, #4357, .T. ) ;
#11390 = DIRECTION ( 'NONE',  ( -0.000000000000000000, -0.000000000000000000, -1.000000000000000000 ) ) ;
#11391 = VERTEX_POINT ( 'NONE', #11206 ) ;
#11392 =( NAMED_UNIT ( * ) SI_UNIT ( $, .STERADIAN. ) SOLID_ANGLE_UNIT ( ) );
#11393 = CARTESIAN_POINT ( 'NONE',  ( 0.000000000000000000, 2.750709400713692965, 33.00000000000012790 ) ) ;
#11394 = LINE ( 'NONE', #7870, #7809 ) ;
#11395 = CARTESIAN_POINT ( 'NONE',  ( 103.2469880950108063, 0.000000000000000000, -33.00000000000012790 ) ) ;
#11396 = ORIENTED_EDGE ( 'NONE', *, *, #663, .F. ) ;
#11397 = DIRECTION ( 'NONE',  ( 1.000000000000000000, 0.000000000000000000, 0.000000000000000000 ) ) ;
#11398 = CARTESIAN_POINT ( 'NONE',  ( -80.00000000000001421, -74.24929059928631148, 4.000000000000000000 ) ) ;
#11399 = CARTESIAN_POINT ( 'NONE',  ( 32.94077818407075853, -56.07092277360308685, 2.830630916608660286 ) ) ;
#11400 = DIRECTION ( 'NONE',  ( 0.000000000000000000, 0.000000000000000000, -1.000000000000000000 ) ) ;
#11401 = CARTESIAN_POINT ( 'NONE',  ( -29.99999999999998579, 23.95881716715919652, 33.00000000000017053 ) ) ;
#11402 = ORIENTED_EDGE ( 'NONE', *, *, #10547, .T. ) ;
#11403 = EDGE_LOOP ( 'NONE', ( #2069, #968, #6030, #5875 ) ) ;
#11404 = CARTESIAN_POINT ( 'NONE',  ( 32.52281604437752804, -59.06479067038042530, 2.757123406423263923 ) ) ;
#11405 = ORIENTED_EDGE ( 'NONE', *, *, #15062, .F. ) ;
#11406 = DIRECTION ( 'NONE',  ( 1.000000000000000000, 1.156482317317871725E-16, 0.000000000000000000 ) ) ;
#11407 = DIRECTION ( 'NONE',  ( 0.000000000000000000, 1.000000000000000000, -0.000000000000000000 ) ) ;
#11408 = ORIENTED_EDGE ( 'NONE', *, *, #4228, .F. ) ;
#11409 = CARTESIAN_POINT ( 'NONE',  ( 109.8334623555409735, 23.25070940071369563, 33.00000000000012790 ) ) ;
#11410 = LINE ( 'NONE', #9204, #15160 ) ;
#11411 = EDGE_CURVE ( 'NONE', #6172, #10924, #966, .T. ) ;
#11412 = DIRECTION ( 'NONE',  ( -0.000000000000000000, 0.000000000000000000, -1.000000000000000000 ) ) ;
#11413 = DIRECTION ( 'NONE',  ( -0.000000000000000000, -0.000000000000000000, -1.000000000000000000 ) ) ;
#11414 = DIRECTION ( 'NONE',  ( 0.000000000000000000, -0.000000000000000000, -1.000000000000000000 ) ) ;
#11415 = DIRECTION ( 'NONE',  ( 1.000000000000000000, 0.000000000000000000, 0.000000000000000000 ) ) ;
#11416 = LINE ( 'NONE', #12509, #10418 ) ;
#11417 = DIRECTION ( 'NONE',  ( -0.000000000000000000, -1.000000000000000000, -0.000000000000000000 ) ) ;
#11418 = ORIENTED_EDGE ( 'NONE', *, *, #7268, .T. ) ;
#11419 = LINE ( 'NONE', #5760, #11960 ) ;
#11420 = VERTEX_POINT ( 'NONE', #2126 ) ;
#11421 = CARTESIAN_POINT ( 'NONE',  ( 50.19487218104683990, 2.077162398607073079, 47.51982618741348574 ) ) ;
#11422 = ORIENTED_EDGE ( 'NONE', *, *, #4415, .F. ) ;
#11423 = DIRECTION ( 'NONE',  ( 0.000000000000000000, 0.000000000000000000, 1.000000000000000000 ) ) ;
#11424 = EDGE_CURVE ( 'NONE', #14061, #9229, #14427, .T. ) ;
#11425 = CYLINDRICAL_SURFACE ( 'NONE', #8751, 4.276034690655513337 ) ;
#11426 = VECTOR ( 'NONE', #5332, 1000.000000000000000 ) ;
#11427 = DIRECTION ( 'NONE',  ( -1.000000000000000000, 0.000000000000000000, 0.000000000000000000 ) ) ;
#11428 = DIRECTION ( 'NONE',  ( 0.8420378618367644341, 0.5394184268574535590, 0.000000000000000000 ) ) ;
#11429 = CARTESIAN_POINT ( 'NONE',  ( 27.85548922659567239, -68.67521603616586390, -4.260811380315422170 ) ) ;
#11430 = VERTEX_POINT ( 'NONE', #734 ) ;
#11431 = APPLICATION_CONTEXT ( 'automotive_design' ) ;
#11432 = CARTESIAN_POINT ( 'NONE',  ( -3.285520523749251520, 5.681530634151883419, -48.00000000000012079 ) ) ;
#11433 = CARTESIAN_POINT ( 'NONE',  ( 8.812572261450901223, -55.94973218888541311, -2.850075077558482661 ) ) ;
#11434 = DIRECTION ( 'NONE',  ( 0.000000000000000000, 0.000000000000000000, 1.000000000000000000 ) ) ;
#11435 = FACE_OUTER_BOUND ( 'NONE', #14036, .T. ) ;
#11436 = EDGE_LOOP ( 'NONE', ( #2188, #7783 ) ) ;
#11437 = B_SPLINE_CURVE_WITH_KNOTS ( 'NONE', 3,
 ( #5784, #11919, #7086, #11771, #8395, #10549 ),
 .UNSPECIFIED., .F., .F.,
 ( 4, 2, 4 ),
 ( 0.000000000000000000, 0.0003908577252344195446, 0.0007817154504688390891 ),
 .UNSPECIFIED. ) ;
#11438 = ORIENTED_EDGE ( 'NONE', *, *, #4617, .T. ) ;
#11439 = AXIS2_PLACEMENT_3D ( 'NONE', #3443, #6984, #1120 ) ;
#11440 = LINE ( 'NONE', #13916, #5116 ) ;
#11441 = ORIENTED_EDGE ( 'NONE', *, *, #8194, .T. ) ;
#11442 = CARTESIAN_POINT ( 'NONE',  ( -2.016677571526633510E-15, 23.25070940071368497, 33.00000000000012790 ) ) ;
#11443 = ORIENTED_EDGE ( 'NONE', *, *, #6370, .T. ) ;
#11444 = CARTESIAN_POINT ( 'NONE',  ( 9.200644618036294631, -59.06479067038042530, -2.757123406423266587 ) ) ;
#11445 = DIRECTION ( 'NONE',  ( 0.000000000000000000, -0.000000000000000000, 1.000000000000000000 ) ) ;
#11446 = ORIENTED_EDGE ( 'NONE', *, *, #339, .F. ) ;
#11447 = VECTOR ( 'NONE', #7081, 1000.000000000000000 ) ;
#11448 = CARTESIAN_POINT ( 'NONE',  ( 10.42235396810873027, -53.71233130651032894, -3.555899869131464719 ) ) ;
#11449 = AXIS2_PLACEMENT_3D ( 'NONE', #10678, #8585, #14372 ) ;
#11450 = CARTESIAN_POINT ( 'NONE',  ( 37.23881781239525424, 0.000000000000000000, -33.00000000000012790 ) ) ;
#11451 = VERTEX_POINT ( 'NONE', #890 ) ;
#11452 = CARTESIAN_POINT ( 'NONE',  ( 62.14609464170151654, 0.6526447315840442354, 48.51982618741349285 ) ) ;
#11453 = CARTESIAN_POINT ( 'NONE',  ( 64.61411691048888883, -11.63232581132101195, 73.01473414043169896 ) ) ;
#11454 = DIRECTION ( 'NONE',  ( -1.000000000000000000, -0.000000000000000000, -0.000000000000000000 ) ) ;
#11455 = AXIS2_PLACEMENT_3D ( 'NONE', #12793, #6851, #5634 ) ;
#11456 = DIRECTION ( 'NONE',  ( 0.7546336727145961376, -0.5961293309129300777, 0.2741493039031510648 ) ) ;
#11457 = CARTESIAN_POINT ( 'NONE',  ( 31.67019424172517716, -63.64653881684405690, 2.711348815098903575 ) ) ;
#11458 = ORIENTED_EDGE ( 'NONE', *, *, #13140, .T. ) ;
#11459 = CARTESIAN_POINT ( 'NONE',  ( 69.28051765693513175, -4.295678830383772961, 71.19766410831373094 ) ) ;
#11460 = ADVANCED_FACE ( 'NONE', ( #7753 ), #5602, .F. ) ;
#11461 = VECTOR ( 'NONE', #7194, 1000.000000000000000 ) ;
#11462 = CIRCLE ( 'NONE', #13420, 9.500000000000001776 ) ;
#11463 = CARTESIAN_POINT ( 'NONE',  ( -8.982583014919022446, 1.839844381040865562, 48.00000000000012079 ) ) ;
#11464 = ORIENTED_EDGE ( 'NONE', *, *, #13049, .F. ) ;
#11465 = LINE ( 'NONE', #5637, #8417 ) ;
#11466 = SHAPE_REPRESENTATION ( 'Bench-Mounted Base Unit', ( #6315 ), #3366 ) ;
#11467 = CYLINDRICAL_SURFACE ( 'NONE', #13185, 0.5000000000000000000 ) ;
#11468 = DIRECTION ( 'NONE',  ( 0.9991708782893151675, -0.04071309345356645404, 0.000000000000000000 ) ) ;
#11469 = CARTESIAN_POINT ( 'NONE',  ( 80.00000000000001421, -87.24929059928631148, -35.00000000000000000 ) ) ;
#11470 = ORIENTED_EDGE ( 'NONE', *, *, #9236, .F. ) ;
#11471 = AXIS2_PLACEMENT_3D ( 'NONE', #6977, #9053, #12831 ) ;
#11472 = DIRECTION ( 'NONE',  ( 0.000000000000000000, 0.000000000000000000, -1.000000000000000000 ) ) ;
#11473 = EDGE_CURVE ( 'NONE', #13714, #931, #5444, .T. ) ;
#11474 = ADVANCED_FACE ( 'NONE', ( #7984 ), #7833, .T. ) ;
#11475 = AXIS2_PLACEMENT_3D ( 'NONE', #2949, #11246, #5406 ) ;
#11476 = DIRECTION ( 'NONE',  ( 0.5394184268574520047, -0.8420378618367654333, 0.000000000000000000 ) ) ;
#11477 = CARTESIAN_POINT ( 'NONE',  ( 13.86173033120691045, -68.61243380581730378, 3.657093847832754818 ) ) ;
#11478 = CARTESIAN_POINT ( 'NONE',  ( 8.948125790170779581, -57.91121052158847249, 2.751677492798614288 ) ) ;
#11479 = CYLINDRICAL_SURFACE ( 'NONE', #12079, 2.499999999999995115 ) ;
#11480 = AXIS2_PLACEMENT_3D ( 'NONE', #4582, #4506, #9283 ) ;
#11481 = ORIENTED_EDGE ( 'NONE', *, *, #14983, .T. ) ;
#11482 = CARTESIAN_POINT ( 'NONE',  ( 32.87342042526285013, -60.00774340954441044, 2.531751357929999280 ) ) ;
#11483 = CIRCLE ( 'NONE', #6339, 3.000000000000000888 ) ;
#11484 = ORIENTED_EDGE ( 'NONE', *, *, #4906, .F. ) ;
#11485 = DIRECTION ( 'NONE',  ( 0.8746197071345573892, -0.4848096202550657985, 0.000000000000000000 ) ) ;
#11486 = CARTESIAN_POINT ( 'NONE',  ( 23.10474973039555380, -52.24929059928630437, 5.564967562786275579 ) ) ;
#11487 = CIRCLE ( 'NONE', #12489, 3.694885682588112896 ) ;
#11488 = VECTOR ( 'NONE', #11633, 1000.000000000000000 ) ;
#11489 = EDGE_LOOP ( 'NONE', ( #5967, #3959 ) ) ;
#11490 = LINE ( 'NONE', #14804, #13814 ) ;
#11491 = DIRECTION ( 'NONE',  ( 0.000000000000000000, 0.000000000000000000, 1.000000000000000000 ) ) ;
#11492 = DIRECTION ( 'NONE',  ( -0.000000000000000000, -1.000000000000000000, -0.000000000000000000 ) ) ;
#11493 = VECTOR ( 'NONE', #13095, 1000.000000000000000 ) ;
#11494 = LINE ( 'NONE', #8122, #3872 ) ;
#11495 = LINE ( 'NONE', #5352, #4360 ) ;
#11496 = FACE_OUTER_BOUND ( 'NONE', #3970, .T. ) ;
#11497 = CIRCLE ( 'NONE', #4376, 4.000000000000003553 ) ;
#11498 = CARTESIAN_POINT ( 'NONE',  ( 20.86173033120691045, -69.39711819508849544, 0.000000000000000000 ) ) ;
#11499 = EDGE_CURVE ( 'NONE', #1741, #12265, #7785, .T. ) ;
#11500 = DIRECTION ( 'NONE',  ( 0.000000000000000000, 0.000000000000000000, 1.000000000000000000 ) ) ;
#11501 = ORIENTED_EDGE ( 'NONE', *, *, #7909, .T. ) ;
#11502 = DIRECTION ( 'NONE',  ( -0.000000000000000000, -0.000000000000000000, -1.000000000000000000 ) ) ;
#11503 = ORIENTED_EDGE ( 'NONE', *, *, #2985, .T. ) ;
#11504 = DIRECTION ( 'NONE',  ( -0.000000000000000000, 1.000000000000000000, 1.445602896647339163E-16 ) ) ;
#11505 = VERTEX_POINT ( 'NONE', #13752 ) ;
#11506 = DIRECTION ( 'NONE',  ( 0.7915791710638007128, 0.6110666215217015473, 0.000000000000000000 ) ) ;
#11507 = CARTESIAN_POINT ( 'NONE',  ( 120.5019411979502451, -32.32126606797570645, 54.40673322733726991 ) ) ;
#11508 = CARTESIAN_POINT ( 'NONE',  ( 80.00000000000001421, -85.24929059928629727, -32.00000000000000000 ) ) ;
#11509 = ORIENTED_EDGE ( 'NONE', *, *, #2453, .T. ) ;
#11510 = CIRCLE ( 'NONE', #11224, 0.5000000000000008882 ) ;
#11511 = CARTESIAN_POINT ( 'NONE',  ( 27.32034923811608707, -68.64054039872385715, -4.542265185079617851 ) ) ;
#11512 = ORIENTED_EDGE ( 'NONE', *, *, #1131, .T. ) ;
#11513 = LINE ( 'NONE', #3369, #8827 ) ;
#11514 = CARTESIAN_POINT ( 'NONE',  ( 8.990114402468742938, -55.34773484034933944, -2.956285999963581101 ) ) ;
#11515 = FACE_OUTER_BOUND ( 'NONE', #14762, .T. ) ;
#11516 = EDGE_CURVE ( 'NONE', #15000, #211, #11716, .T. ) ;
#11517 = EDGE_CURVE ( 'NONE', #6801, #3301, #12741, .T. ) ;
#11518 = DIRECTION ( 'NONE',  ( 0.000000000000000000, 0.000000000000000000, 1.000000000000000000 ) ) ;
#11519 = AXIS2_PLACEMENT_3D ( 'NONE', #6208, #12261, #1716 ) ;
#11520 = VERTEX_POINT ( 'NONE', #10062 ) ;
#11521 = CARTESIAN_POINT ( 'NONE',  ( 63.55116547662790794, -2.088839582009629936, 60.61639468829817190 ) ) ;
#11522 = ORIENTED_EDGE ( 'NONE', *, *, #1739, .F. ) ;
#11523 = LINE ( 'NONE', #6607, #1538 ) ;
#11524 = ORIENTED_EDGE ( 'NONE', *, *, #2520, .T. ) ;
#11525 = EDGE_CURVE ( 'NONE', #10265, #3380, #10244, .T. ) ;
#11526 = CARTESIAN_POINT ( 'NONE',  ( 80.00000000000001421, -85.24929059928629727, -32.00000000000000000 ) ) ;
#11527 = CARTESIAN_POINT ( 'NONE',  ( -23.72465974793126620, 3.743354278179100714, -47.97348817130775700 ) ) ;
#11528 = LINE ( 'NONE', #985, #5204 ) ;
#11529 = FACE_OUTER_BOUND ( 'NONE', #4492, .T. ) ;
#11530 = ORIENTED_EDGE ( 'NONE', *, *, #4655, .T. ) ;
#11531 = EDGE_CURVE ( 'NONE', #81, #1671, #13671, .T. ) ;
#11532 = LINE ( 'NONE', #14167, #13707 ) ;
#11533 = CARTESIAN_POINT ( 'NONE',  ( 80.00000000000001421, -74.24929059928631148, 32.99999999999999289 ) ) ;
#11534 = CARTESIAN_POINT ( 'NONE',  ( 69.46373470288038732, -2.401743389192480649, 75.84280485847520481 ) ) ;
#11535 = DIRECTION ( 'NONE',  ( 0.000000000000000000, 0.000000000000000000, 1.000000000000000000 ) ) ;
#11536 = CARTESIAN_POINT ( 'NONE',  ( 24.14199725329817880, -70.03159917007936031, 6.184016381206977719 ) ) ;
#11537 = EDGE_LOOP ( 'NONE', ( #1749, #9642, #9912, #10364 ) ) ;
#11538 = LINE ( 'NONE', #9479, #12746 ) ;
#11539 = VECTOR ( 'NONE', #8500, 1000.000000000000000 ) ;
#11540 = CARTESIAN_POINT ( 'NONE',  ( 18.24487436548682595, -52.24929059928630437, 6.492462156583967747 ) ) ;
#11541 = VERTEX_POINT ( 'NONE', #815 ) ;
#11542 = DIRECTION ( 'NONE',  ( 1.000000000000000000, 1.110223024625156540E-15, -0.000000000000000000 ) ) ;
#11543 = DIRECTION ( 'NONE',  ( -0.000000000000000000, -0.000000000000000000, 1.000000000000000000 ) ) ;
#11544 = VERTEX_POINT ( 'NONE', #1824 ) ;
#11545 =( NAMED_UNIT ( * ) SI_UNIT ( $, .STERADIAN. ) SOLID_ANGLE_UNIT ( ) );
#11546 = CARTESIAN_POINT ( 'NONE',  ( -80.00000000000001421, -72.24929059928631148, 32.99999999999999289 ) ) ;
#11547 = CARTESIAN_POINT ( 'NONE',  ( -20.99999999999998579, -2.249290599286303927, 33.00000000000012790 ) ) ;
#11548 = ORIENTED_EDGE ( 'NONE', *, *, #6285, .T. ) ;
#11549 = DIRECTION ( 'NONE',  ( 0.000000000000000000, 1.000000000000000000, 0.000000000000000000 ) ) ;
#11550 = DIRECTION ( 'NONE',  ( 1.000000000000000000, 0.000000000000000000, 0.000000000000000000 ) ) ;
#11551 = AXIS2_PLACEMENT_3D ( 'NONE', #10925, #7378, #10767 ) ;
#11552 = CARTESIAN_POINT ( 'NONE',  ( 70.26445833701072274, -4.474174595298148205, 77.19766410831374515 ) ) ;
#11553 = DIRECTION ( 'NONE',  ( -0.8746197071345569451, 0.4848096202550666312, 0.000000000000000000 ) ) ;
#11554 = DIRECTION ( 'NONE',  ( 0.000000000000000000, 0.000000000000000000, 1.000000000000000000 ) ) ;
#11555 = DIRECTION ( 'NONE',  ( -0.000000000000000000, -0.000000000000000000, -1.000000000000000000 ) ) ;
#11556 = B_SPLINE_CURVE_WITH_KNOTS ( 'NONE', 3,
 ( #5041, #5334, #1646, #6345, #14501, #5183, #627, #414 ),
 .UNSPECIFIED., .F., .F.,
 ( 4, 2, 2, 4 ),
 ( 0.000000000000000000, 0.0002685268308981138730, 0.0005370536617962277460, 0.001074107323592453107 ),
 .UNSPECIFIED. ) ;
#11557 = EDGE_CURVE ( 'NONE', #11277, #10236, #14190, .T. ) ;
#11558 = ORIENTED_EDGE ( 'NONE', *, *, #13741, .T. ) ;
#11559 = AXIS2_PLACEMENT_3D ( 'NONE', #1901, #13310, #6380 ) ;
#11560 = CARTESIAN_POINT ( 'NONE',  ( 31.49298359385885959, -60.71197230342421136, 3.050751728647424610 ) ) ;
#11561 = ORIENTED_EDGE ( 'NONE', *, *, #5470, .F. ) ;
#11562 = EDGE_CURVE ( 'NONE', #10924, #11787, #181, .T. ) ;
#11563 = DIRECTION ( 'NONE',  ( 0.000000000000000000, 1.000000000000000000, 0.000000000000000000 ) ) ;
#11564 = FACE_OUTER_BOUND ( 'NONE', #6658, .T. ) ;
#11565 = ORIENTED_EDGE ( 'NONE', *, *, #14279, .F. ) ;
#11566 = ADVANCED_FACE ( 'NONE', ( #7907 ), #6591, .T. ) ;
#11567 = ADVANCED_FACE ( 'NONE', ( #6743 ), #2035, .F. ) ;
#11568 = ORIENTED_EDGE ( 'NONE', *, *, #2311, .F. ) ;
#11569 = FACE_OUTER_BOUND ( 'NONE', #7777, .T. ) ;
#11570 = DIRECTION ( 'NONE',  ( -0.5006040828730976555, 0.8656763553492637930, 0.000000000000000000 ) ) ;
#11571 = CIRCLE ( 'NONE', #8866, 2.524999999999999467 ) ;
#11572 = FACE_OUTER_BOUND ( 'NONE', #8229, .T. ) ;
#11573 = EDGE_CURVE ( 'NONE', #11128, #4675, #2132, .T. ) ;
#11574 = CIRCLE ( 'NONE', #8398, 0.7892041907098262810 ) ;
#11575 = CARTESIAN_POINT ( 'NONE',  ( -16.99999999999998579, -2.249290599286305703, -32.99999999999987921 ) ) ;
#11576 = FACE_OUTER_BOUND ( 'NONE', #8526, .T. ) ;
#11577 = LINE ( 'NONE', #10127, #14037 ) ;
#11578 = B_SPLINE_CURVE_WITH_KNOTS ( 'NONE', 3,
 ( #9976, #6429, #13661, #7664 ),
 .UNSPECIFIED., .F., .F.,
 ( 4, 4 ),
 ( 0.0005996816226311996569, 0.004245596575621808817 ),
 .UNSPECIFIED. ) ;
#11579 = DIRECTION ( 'NONE',  ( -0.000000000000000000, 0.000000000000000000, 1.000000000000000000 ) ) ;
#11580 = DIRECTION ( 'NONE',  ( -0.3351302520855081735, 0.000000000000000000, 0.9421718071228324387 ) ) ;
#11581 = ORIENTED_EDGE ( 'NONE', *, *, #8512, .F. ) ;
#11582 = CARTESIAN_POINT ( 'NONE',  ( 10.05326642068865262, -63.64653881684382952, -2.711348815098831633 ) ) ;
#11583 = VECTOR ( 'NONE', #11881, 1000.000000000000000 ) ;
#11584 = CIRCLE ( 'NONE', #3239, 9.000000000000001776 ) ;
#11585 = ORIENTED_EDGE ( 'NONE', *, *, #14309, .F. ) ;
#11586 = DIRECTION ( 'NONE',  ( -0.000000000000000000, -0.000000000000000000, -1.000000000000000000 ) ) ;
#11587 = AXIS2_PLACEMENT_3D ( 'NONE', #13772, #12786, #4457 ) ;
#11588 = VERTEX_POINT ( 'NONE', #9742 ) ;
#11589 = SURFACE_SIDE_STYLE ('',( #8134 ) ) ;
#11590 = ADVANCED_FACE ( 'NONE', ( #1417 ), #14425, .F. ) ;
#11591 = DIRECTION ( 'NONE',  ( 1.000000000000000000, 0.000000000000000000, 0.000000000000000000 ) ) ;
#11592 = CARTESIAN_POINT ( 'NONE',  ( 58.00000000000000711, -2.249290599286309256, 87.40005259842790508 ) ) ;
#11593 = DIRECTION ( 'NONE',  ( 0.000000000000000000, 0.000000000000000000, 1.000000000000000000 ) ) ;
#11594 = VECTOR ( 'NONE', #2843, 1000.000000000000000 ) ;
#11595 = ORIENTED_EDGE ( 'NONE', *, *, #15099, .F. ) ;
#11596 = AXIS2_PLACEMENT_3D ( 'NONE', #7387, #14947, #13868 ) ;
#11597 = CARTESIAN_POINT ( 'NONE',  ( -3.190546569013415379, 0.8906624217387615339, -57.50000000000012079 ) ) ;
#11598 = CARTESIAN_POINT ( 'NONE',  ( 8.286281640854550545, -55.20947656326016073, -1.969991847666946905 ) ) ;
#11599 = DIRECTION ( 'NONE',  ( 1.000000000000000000, 0.000000000000000000, 0.000000000000000000 ) ) ;
#11600 = CARTESIAN_POINT ( 'NONE',  ( 76.14589960879430919, -7.734310727912411920, 76.19766410831374515 ) ) ;
#11601 = ORIENTED_EDGE ( 'NONE', *, *, #5311, .T. ) ;
#11602 = ORIENTED_EDGE ( 'NONE', *, *, #2263, .F. ) ;
#11603 = LINE ( 'NONE', #6233, #12967 ) ;
#11604 = ORIENTED_EDGE ( 'NONE', *, *, #3799, .F. ) ;
#11605 = LINE ( 'NONE', #11442, #11113 ) ;
#11606 = EDGE_CURVE ( 'NONE', #12694, #12778, #8279, .T. ) ;
#11607 = ORIENTED_EDGE ( 'NONE', *, *, #7012, .T. ) ;
#11608 = CIRCLE ( 'NONE', #3251, 0.7892041907098262810 ) ;
#11609 = VERTEX_POINT ( 'NONE', #6124 ) ;
#11610 = AXIS2_PLACEMENT_3D ( 'NONE', #1322, #14258, #3705 ) ;
#11611 = LINE ( 'NONE', #14004, #9508 ) ;
#11612 = FACE_OUTER_BOUND ( 'NONE', #11, .T. ) ;
#11614 = EDGE_CURVE ( 'NONE', #5061, #3925, #5977, .T. ) ;
#11613 = ORIENTED_EDGE ( 'NONE', *, *, #4092, .T. ) ;
#11615 = EDGE_CURVE ( 'NONE', #14077, #12875, #11888, .T. ) ;
#11616 = FACE_OUTER_BOUND ( 'NONE', #10784, .T. ) ;
#11617 = CARTESIAN_POINT ( 'NONE',  ( 80.18290120114222930, 23.25070940071369208, -33.00000000000012790 ) ) ;
#11618 = ORIENTED_EDGE ( 'NONE', *, *, #2739, .F. ) ;
#11619 = DIRECTION ( 'NONE',  ( 1.000000000000000000, 0.000000000000000000, 0.000000000000000000 ) ) ;
#11620 = CARTESIAN_POINT ( 'NONE',  ( 65.13162939602317181, -11.91918766459985513, 73.19766410831374515 ) ) ;
#11621 = CARTESIAN_POINT ( 'NONE',  ( 18.24487436548682950, -53.24929059928630437, -6.492462156583989064 ) ) ;
#11622 = CARTESIAN_POINT ( 'NONE',  ( 28.85634326780420267, -53.69151354803189946, 4.215873133687699337 ) ) ;
#11623 = VERTEX_POINT ( 'NONE', #10810 ) ;
#11624 = CIRCLE ( 'NONE', #4999, 0.7892041907098262810 ) ;
#11625 = CARTESIAN_POINT ( 'NONE',  ( -9.037775043065350289, 2.932694901963889933, 48.50000000000012079 ) ) ;
#11626 = AXIS2_PLACEMENT_3D ( 'NONE', #13019, #6250, #9477 ) ;
#11627 = ORIENTED_EDGE ( 'NONE', *, *, #3690, .T. ) ;
#11628 = LINE ( 'NONE', #14020, #1272 ) ;
#11629 = SURFACE_SIDE_STYLE ('',( #4633 ) ) ;
#11630 = EDGE_CURVE ( 'NONE', #9272, #8897, #10983, .T. ) ;
#11631 = EDGE_CURVE ( 'NONE', #14830, #6001, #3723, .T. ) ;
#11632 =( NAMED_UNIT ( * ) SI_UNIT ( $, .STERADIAN. ) SOLID_ANGLE_UNIT ( ) );
#11633 = DIRECTION ( 'NONE',  ( -0.000000000000000000, 1.000000000000000000, -0.000000000000000000 ) ) ;
#11634 = CARTESIAN_POINT ( 'NONE',  ( 30.60592481596644632, -62.41236107492795782, 2.580051240451675554 ) ) ;
#11635 = ORIENTED_EDGE ( 'NONE', *, *, #5264, .T. ) ;
#11636 = PRODUCT_RELATED_PRODUCT_CATEGORY ( 'part', '', ( #10155 ) ) ;
#11637 = DIRECTION ( 'NONE',  ( -0.000000000000000000, -0.000000000000000000, -1.000000000000000000 ) ) ;
#11638 = CIRCLE ( 'NONE', #11884, 0.7892041907098261699 ) ;
#11639 = FACE_OUTER_BOUND ( 'NONE', #456, .T. ) ;
#11640 = AXIS2_PLACEMENT_3D ( 'NONE', #670, #10149, #14606 ) ;
#11641 = PLANE ( 'NONE',  #10029 ) ;
#11642 = CYLINDRICAL_SURFACE ( 'NONE', #10056, 0.7892041907098262810 ) ;
#11643 = CARTESIAN_POINT ( 'NONE',  ( 23.69232253801246557, -82.24929059928629727, -4.472107801411126182 ) ) ;
#11644 = DIRECTION ( 'NONE',  ( -0.8746197071345569451, 0.4848096202550666312, 0.000000000000000000 ) ) ;
#11645 = ORIENTED_EDGE ( 'NONE', *, *, #8411, .T. ) ;
#11646 = DIRECTION ( 'NONE',  ( -0.3020115420618265656, 0.1674077314120193949, -0.9384901064608611732 ) ) ;
#11647 = VERTEX_POINT ( 'NONE', #10103 ) ;
#11648 = CARTESIAN_POINT ( 'NONE',  ( 10.49322424505076690, -52.67209071833767808, -2.680141711508894353 ) ) ;
#11649 = CARTESIAN_POINT ( 'NONE',  ( 10.49550990701181696, -52.67117483538238787, 2.680786716676139214 ) ) ;
#11650 = EDGE_LOOP ( 'NONE', ( #2496, #13568, #8337, #11154, #5188 ) ) ;
#11651 = FACE_OUTER_BOUND ( 'NONE', #11684, .T. ) ;
#11652 = DIRECTION ( 'NONE',  ( 0.000000000000000000, -1.000000000000000000, 0.000000000000000000 ) ) ;
#11653 =( REPRESENTATION_RELATIONSHIP ('NONE','NONE', #15125, #2630 ) REPRESENTATION_RELATIONSHIP_WITH_TRANSFORMATION ( #5020 )SHAPE_REPRESENTATION_RELATIONSHIP( ) );
#11654 =( NAMED_UNIT ( * ) PLANE_ANGLE_UNIT ( ) SI_UNIT ( $, .RADIAN. ) );
#11655 = DIRECTION ( 'NONE',  ( 0.000000000000000000, 0.000000000000000000, 1.000000000000000000 ) ) ;
#11656 = CARTESIAN_POINT ( 'NONE',  ( 20.86173033120691045, -69.39711819508849544, 0.000000000000000000 ) ) ;
#11657 = CARTESIAN_POINT ( 'NONE',  ( -2.016677571526633510E-15, 23.25070940071368497, -33.00000000000012790 ) ) ;
#11658 = CARTESIAN_POINT ( 'NONE',  ( 9.286411473068065803, -59.38916093354925607, 2.764669745501079579 ) ) ;
#11659 = CARTESIAN_POINT ( 'NONE',  ( 30.85913393947397054, -53.50034303113434930, 3.720434809418716515 ) ) ;
#11660 = EDGE_CURVE ( 'NONE', #3099, #931, #3613, .T. ) ;
#11661 = EDGE_LOOP ( 'NONE', ( #14916, #314, #1799, #8515 ) ) ;
#11662 = DIRECTION ( 'NONE',  ( 0.000000000000000000, 0.000000000000000000, 1.000000000000000000 ) ) ;
#11663 = UNCERTAINTY_MEASURE_WITH_UNIT (LENGTH_MEASURE( 1.000000000000000082E-05 ), #14044, 'distance_accuracy_value', 'NONE');
#11664 = EDGE_CURVE ( 'NONE', #13577, #13900, #2864, .T. ) ;
#11665 = VERTEX_POINT ( 'NONE', #557 ) ;
#11666 = EDGE_CURVE ( 'NONE', #14080, #531, #13637, .T. ) ;
#11667 = DIRECTION ( 'NONE',  ( 0.000000000000000000, 1.000000000000000000, 0.000000000000000000 ) ) ;
#11668 = VERTEX_POINT ( 'NONE', #9816 ) ;
#11669 = CARTESIAN_POINT ( 'NONE',  ( 14.30639712155258003, -67.71210253279622293, -4.528315385689293926 ) ) ;
#11670 = VERTEX_POINT ( 'NONE', #12407 ) ;
#11671 = DIRECTION ( 'NONE',  ( 1.000000000000000000, 1.156482317317870492E-16, 0.000000000000000000 ) ) ;
#11672 = LINE ( 'NONE', #2363, #12195 ) ;
#11673 = CARTESIAN_POINT ( 'NONE',  ( -80.00000000000001421, -76.24929059928631148, -4.000000000000000000 ) ) ;
#11674 = ORIENTED_EDGE ( 'NONE', *, *, #12243, .F. ) ;
#11675 = ORIENTED_EDGE ( 'NONE', *, *, #10082, .F. ) ;
#11676 = EDGE_CURVE ( 'NONE', #3217, #10912, #10224, .T. ) ;
#11677 = EDGE_CURVE ( 'NONE', #5032, #3522, #12490, .T. ) ;
#11678 = LINE ( 'NONE', #2445, #10608 ) ;
#11679 = CARTESIAN_POINT ( 'NONE',  ( 9.438813863662174342, -53.39687877504488966, -3.230473295589093130 ) ) ;
#11680 = DIRECTION ( 'NONE',  ( 1.000000000000000000, 0.000000000000000000, -9.912705577010325549E-17 ) ) ;
#11681 = DIRECTION ( 'NONE',  ( 0.000000000000000000, 1.000000000000000000, -0.000000000000000000 ) ) ;
#11682 = ORIENTED_EDGE ( 'NONE', *, *, #6455, .T. ) ;
#11683 = LINE ( 'NONE', #9157, #4593 ) ;
#11684 = EDGE_LOOP ( 'NONE', ( #7353, #10884, #9646, #11811 ) ) ;
#11685 = DIRECTION ( 'NONE',  ( -1.000000000000000000, -0.000000000000000000, -0.000000000000000000 ) ) ;
#11686 = VERTEX_POINT ( 'NONE', #483 ) ;
#11687 = ORIENTED_EDGE ( 'NONE', *, *, #4716, .T. ) ;
#11688 = LINE ( 'NONE', #1300, #7050 ) ;
#11689 = LINE ( 'NONE', #8322, #13820 ) ;
#11690 = CARTESIAN_POINT ( 'NONE',  ( 130.4454129427046496, 23.25070940071369563, 13.14990448602692474 ) ) ;
#11691 = DIRECTION ( 'NONE',  ( -0.000000000000000000, 0.000000000000000000, -1.000000000000000000 ) ) ;
#11692 = ORIENTED_EDGE ( 'NONE', *, *, #4119, .T. ) ;
#11693 = TOROIDAL_SURFACE ( 'NONE', #15139, 5.165819364273509073, 0.5000000000000000000 ) ;
#11694 = CARTESIAN_POINT ( 'NONE',  ( 118.0000000000000568, 2.046973701652633381E-13, -13.14990448602693007 ) ) ;
#11695 = CARTESIAN_POINT ( 'NONE',  ( 65.17358638046424346, -11.90957281131293932, 72.92467134341568169 ) ) ;
#11696 = CARTESIAN_POINT ( 'NONE',  ( 47.27423575335444639, 23.25070940071368852, -33.00000000000012790 ) ) ;
#11697 = CARTESIAN_POINT ( 'NONE',  ( 23.53111059738935040, -55.08889408822823697, 6.471126372660433113 ) ) ;
#11698 = ORIENTED_EDGE ( 'NONE', *, *, #15129, .F. ) ;
#11699 = DIRECTION ( 'NONE',  ( 0.8746197071345563900, -0.4848096202550675193, 0.000000000000000000 ) ) ;
#11700 = EDGE_CURVE ( 'NONE', #8652, #5446, #7045, .T. ) ;
#11701 = EDGE_CURVE ( 'NONE', #12443, #3972, #8946, .T. ) ;
#11702 = ORIENTED_EDGE ( 'NONE', *, *, #5178, .T. ) ;
#11703 = CYLINDRICAL_SURFACE ( 'NONE', #2762, 4.505436745857433145 ) ;
#11704 = DIRECTION ( 'NONE',  ( -0.8208219420614780715, 0.4549890321264283277, 0.3453061251629916950 ) ) ;
#11705 = ORIENTED_EDGE ( 'NONE', *, *, #13097, .F. ) ;
#11706 = MECHANICAL_DESIGN_GEOMETRIC_PRESENTATION_REPRESENTATION (  '', ( #7039 ), #13915 ) ;
#11707 = DIRECTION ( 'NONE',  ( 1.000000000000000000, 0.000000000000000000, 0.000000000000000000 ) ) ;
#11708 = CARTESIAN_POINT ( 'NONE',  ( -10.96079405803985729, -9.021238043844263643, -48.26696389624903816 ) ) ;
#11709 = CARTESIAN_POINT ( 'NONE',  ( 28.56964104117922076, -65.59433601606471598, 3.409308316089453506 ) ) ;
#11710 = ORIENTED_EDGE ( 'NONE', *, *, #3896, .F. ) ;
#11711 = CARTESIAN_POINT ( 'NONE',  ( 118.0000000000000284, 19.25070940071370273, 139.1143251403882459 ) ) ;
#11712 = FACE_OUTER_BOUND ( 'NONE', #13370, .T. ) ;
#11713 = FACE_OUTER_BOUND ( 'NONE', #14083, .T. ) ;
#11714 = CARTESIAN_POINT ( 'NONE',  ( -65.00000000000001421, -85.27429059928628874, -17.49999999999999645 ) ) ;
#11715 = DIRECTION ( 'NONE',  ( 0.5006040828730242698, -0.8656763553493062036, 0.000000000000000000 ) ) ;
#11716 = CIRCLE ( 'NONE', #412, 1.000000000000002665 ) ;
#11717 = DIRECTION ( 'NONE',  ( 0.000000000000000000, 0.000000000000000000, -1.000000000000000000 ) ) ;
#11718 = AXIS2_PLACEMENT_3D ( 'NONE', #14143, #3591, #8454 ) ;
#11719 = EDGE_CURVE ( 'NONE', #1828, #302, #82, .T. ) ;
#11720 = VERTEX_POINT ( 'NONE', #5112 ) ;
#11721 = DIRECTION ( 'NONE',  ( 1.000000000000000000, 0.000000000000000000, 0.000000000000000000 ) ) ;
#11722 = CIRCLE ( 'NONE', #6078, 0.5000000000000004441 ) ;
#11723 = VERTEX_POINT ( 'NONE', #4165 ) ;
#11724 = CARTESIAN_POINT ( 'NONE',  ( 8.989437364795538343, -53.88923483553375604, -2.226753743598178570 ) ) ;
#11725 = CARTESIAN_POINT ( 'NONE',  ( 65.00000000000001421, -85.24929059928629727, -17.47499999999999787 ) ) ;
#11726 = AXIS2_PLACEMENT_3D ( 'NONE', #3401, #14103, #3635 ) ;
#11727 = ORIENTED_EDGE ( 'NONE', *, *, #12947, .T. ) ;
#11728 = CARTESIAN_POINT ( 'NONE',  ( -8.842479278987921631, -7.118053859731281463, 48.00000000000012079 ) ) ;
#11729 = LINE ( 'NONE', #2648, #10006 ) ;
#11730 = B_SPLINE_CURVE_WITH_KNOTS ( 'NONE', 3,
 ( #13955, #2251, #10184, #12891, #6951, #4640, #1092, #5803 ),
 .UNSPECIFIED., .F., .F.,
 ( 4, 2, 2, 4 ),
 ( 1.788112030672749005E-18, 0.0006709104321108792356, 0.001341820864221756737, 0.002683641728443497427 ),
 .UNSPECIFIED. ) ;
#11731 = AXIS2_PLACEMENT_3D ( 'NONE', #697, #2860, #8568 ) ;
#11732 = DIRECTION ( 'NONE',  ( 0.4848096202550659650, 0.8746197071345572782, 0.000000000000000000 ) ) ;
#11733 = CARTESIAN_POINT ( 'NONE',  ( -20.99999999999998579, -2.249290599286303927, 36.00000000000012079 ) ) ;
#11734 = CYLINDRICAL_SURFACE ( 'NONE', #14698, 4.665819364273509073 ) ;
#11735 = CARTESIAN_POINT ( 'NONE',  ( 55.36337191871069763, -7.136966431295542534, 54.56811043785582882 ) ) ;
#11736 = AXIS2_PLACEMENT_3D ( 'NONE', #9763, #13291, #5205 ) ;
#11737 = ADVANCED_FACE ( 'NONE', ( #11101 ), #14498, .F. ) ;
#11738 = CARTESIAN_POINT ( 'NONE',  ( 9.665531796221262795, -60.12744825561600948, 2.859530283892859348 ) ) ;
#11739 = VECTOR ( 'NONE', #12318, 1000.000000000000000 ) ;
#11740 = CARTESIAN_POINT ( 'NONE',  ( 32.73334625994522185, -55.34773484034921864, 2.956285999963537581 ) ) ;
#11741 = VERTEX_POINT ( 'NONE', #11175 ) ;
#11742 = VECTOR ( 'NONE', #6028, 1000.000000000000000 ) ;
#11743 = FACE_OUTER_BOUND ( 'NONE', #13460, .T. ) ;
#11744 = ORIENTED_EDGE ( 'NONE', *, *, #11145, .T. ) ;
#11745 = CARTESIAN_POINT ( 'NONE',  ( 98.40734512546775647, 0.000000000000000000, 33.00000000000012790 ) ) ;
#11746 = ORIENTED_EDGE ( 'NONE', *, *, #9136, .F. ) ;
#11747 = ORIENTED_EDGE ( 'NONE', *, *, #14094, .T. ) ;
#11748 = DIRECTION ( 'NONE',  ( 0.8746197071345582774, -0.4848096202550639666, 0.000000000000000000 ) ) ;
#11749 = CARTESIAN_POINT ( 'NONE',  ( 20.86173033120691045, -85.24929059928631148, 0.000000000000000000 ) ) ;
#11750 = VECTOR ( 'NONE', #6620, 1000.000000000000000 ) ;
#11751 = CARTESIAN_POINT ( 'NONE',  ( 14.09856246968317528, -52.24929059928631148, -4.899481419395764981 ) ) ;
#11752 = ADVANCED_FACE ( 'NONE', ( #14635 ), #3090, .T. ) ;
#11753 = AXIS2_PLACEMENT_3D ( 'NONE', #4419, #8964, #6887 ) ;
#11754 = ORIENTED_EDGE ( 'NONE', *, *, #1843, .F. ) ;
#11755 = CARTESIAN_POINT ( 'NONE',  ( 32.39917484285220439, 0.000000000000000000, -33.00000000000012790 ) ) ;
#11756 = DIRECTION ( 'NONE',  ( -0.5394184268574385710, 0.8420378618367740930, 0.000000000000000000 ) ) ;
#11757 = DIRECTION ( 'NONE',  ( -0.000000000000000000, -0.000000000000000000, -1.000000000000000000 ) ) ;
#11758 = ORIENTED_EDGE ( 'NONE', *, *, #10001, .T. ) ;
#11759 = ORIENTED_EDGE ( 'NONE', *, *, #14969, .T. ) ;
#11760 = CARTESIAN_POINT ( 'NONE',  ( 32.77533165178194707, -57.91122518709860856, 2.751677560523507982 ) ) ;
#11761 = ORIENTED_EDGE ( 'NONE', *, *, #364, .F. ) ;
#11762 = CARTESIAN_POINT ( 'NONE',  ( 10.23047706855496841, -60.71197230342421136, 3.050751728647412175 ) ) ;
#11763 = ORIENTED_EDGE ( 'NONE', *, *, #4031, .T. ) ;
#11764 = EDGE_LOOP ( 'NONE', ( #12761, #2085, #10967, #8796 ) ) ;
#11765 = EDGE_CURVE ( 'NONE', #5614, #9539, #6486, .T. ) ;
#11766 = EDGE_CURVE ( 'NONE', #10853, #15152, #8865, .T. ) ;
#11767 = EDGE_CURVE ( 'NONE', #11668, #11983, #5643, .T. ) ;
#11768 = CARTESIAN_POINT ( 'NONE',  ( -24.72817752516938228, 2.363221963240404566, -47.50000000000012079 ) ) ;
#11769 = LINE ( 'NONE', #5932, #11348 ) ;
#11770 = DIRECTION ( 'NONE',  ( 0.000000000000000000, 1.000000000000000000, -0.000000000000000000 ) ) ;
#11771 = CARTESIAN_POINT ( 'NONE',  ( -8.655068852960594583, 2.300722221922764543, 48.05421924268924272 ) ) ;
#11772 = ORIENTED_EDGE ( 'NONE', *, *, #13202, .F. ) ;
#11773 = ADVANCED_FACE ( 'NONE', ( #3407 ), #11693, .T. ) ;
#11774 = CARTESIAN_POINT ( 'NONE',  ( 80.18290120114222930, 29.52935533987996664, 21.00807340887166674 ) ) ;
#11775 = CARTESIAN_POINT ( 'NONE',  ( -9.456839514482961562, 2.659958822950721835, -48.50000000000012079 ) ) ;
#11776 = CARTESIAN_POINT ( 'NONE',  ( -24.96222495693456978, -7.431276100536581275, -58.00000000000012079 ) ) ;
#11777 = ORIENTED_EDGE ( 'NONE', *, *, #5459, .F. ) ;
#11778 = DIRECTION ( 'NONE',  ( -0.3351302520855081735, 0.000000000000000000, -0.9421718071228324387 ) ) ;
#11779 = ORIENTED_EDGE ( 'NONE', *, *, #9981, .T. ) ;
#11780 = CARTESIAN_POINT ( 'NONE',  ( 58.80593636315131079, 3.245402227105440129, 54.56811043785582882 ) ) ;
#11781 = CIRCLE ( 'NONE', #13261, 0.9999999999999957812 ) ;
#11782 = CIRCLE ( 'NONE', #5148, 4.999999999999997335 ) ;
#11783 = ORIENTED_EDGE ( 'NONE', *, *, #12051, .T. ) ;
#11784 = ORIENTED_EDGE ( 'NONE', *, *, #949, .T. ) ;
#11785 = FACE_OUTER_BOUND ( 'NONE', #10340, .T. ) ;
#11786 = DIRECTION ( 'NONE',  ( -0.8746197071345569451, 0.4848096202550666312, 0.000000000000000000 ) ) ;
#11787 = VERTEX_POINT ( 'NONE', #8102 ) ;
#11788 = DIRECTION ( 'NONE',  ( -0.000000000000000000, -0.000000000000000000, 1.000000000000000000 ) ) ;
#11789 = B_SPLINE_CURVE_WITH_KNOTS ( 'NONE', 3,
 ( #8116, #14962, #6799, #1025, #1945, #13648, #9270, #12816, #3267, #13965, #9200, #2262, #11649, #945, #5419, #12739, #5657, #5506 ),
 .UNSPECIFIED., .F., .F.,
 ( 4, 2, 2, 2, 2, 2, 2, 2, 4 ),
 ( 0.0009656645577509051157, 0.001819362422807364790, 0.002673060287863824463, 0.003526758152920284571, 0.004380456017976744679, 0.005234153883033203919, 0.006087851748089664027, 0.006941549613146123267, 0.007795247478202583374 ),
 .UNSPECIFIED. ) ;
#11790 = FACE_OUTER_BOUND ( 'NONE', #6518, .T. ) ;
#11791 = DIRECTION ( 'NONE',  ( -0.000000000000000000, 0.000000000000000000, -1.000000000000000000 ) ) ;
#11792 = CARTESIAN_POINT ( 'NONE',  ( 29.49572703012646357, -62.74876579108524766, 3.782929430830329842 ) ) ;
#11793 = CARTESIAN_POINT ( 'NONE',  ( 0.6601805061683232445, -1.030548743169294346, -57.50000000000012079 ) ) ;
#11794 = AXIS2_PLACEMENT_3D ( 'NONE', #10591, #13055, #5909 ) ;
#11795 = CARTESIAN_POINT ( 'NONE',  ( 31.31200846133606319, -52.71989690418642027, -2.656489712860274466 ) ) ;
#11796 = ORIENTED_EDGE ( 'NONE', *, *, #5463, .T. ) ;
#11797 = CARTESIAN_POINT ( 'NONE',  ( -25.01741698508091005, -6.338425579613558014, -47.50000000000012079 ) ) ;
#11798 = VERTEX_POINT ( 'NONE', #1011 ) ;
#11799 = DIRECTION ( 'NONE',  ( -1.000000000000000000, -8.673617379884035472E-17, 0.000000000000000000 ) ) ;
#11800 = CARTESIAN_POINT ( 'NONE',  ( 18.08359295236611786, -58.63441909321034728, 6.426091441073436883 ) ) ;
#11801 = LINE ( 'NONE', #4806, #7301 ) ;
#11802 = DIRECTION ( 'NONE',  ( 0.2245716668862459686, -0.9744202983869693080, 0.008523410314123252077 ) ) ;
#11803 = CIRCLE ( 'NONE', #11297, 12.46463184759104870 ) ;
#11804 = CARTESIAN_POINT ( 'NONE',  ( 69.46156643657255358, -2.520042852607651263, 76.11175476292719111 ) ) ;
#11805 = EDGE_CURVE ( 'NONE', #13383, #14721, #4638, .T. ) ;
#11806 = ADVANCED_FACE ( 'NONE', ( #12723 ), #6863, .F. ) ;
#11807 = DIRECTION ( 'NONE',  ( -1.000000000000000000, -0.000000000000000000, -0.000000000000000000 ) ) ;
#11808 = CARTESIAN_POINT ( 'NONE',  ( -24.54316048551696028, -7.158540021523408292, 48.50000000000011369 ) ) ;
#11809 = CARTESIAN_POINT ( 'NONE',  ( 80.00000000000001421, -87.24929059928631148, 35.00000000000000000 ) ) ;
#11810 = CARTESIAN_POINT ( 'NONE',  ( 33.47477952685317604, -55.33002571195186903, 2.691408569078770796 ) ) ;
#11811 = ORIENTED_EDGE ( 'NONE', *, *, #12380, .F. ) ;
#11812 = ADVANCED_BREP_SHAPE_REPRESENTATION ( '', ( #14540, #6315 ), #5577 ) ;
#11813 = FACE_OUTER_BOUND ( 'NONE', #5449, .T. ) ;
#11814 = ORIENTED_EDGE ( 'NONE', *, *, #7758, .F. ) ;
#11815 = DIRECTION ( 'NONE',  ( 0.000000000000000000, -0.000000000000000000, 1.000000000000000000 ) ) ;
#11816 = ORIENTED_EDGE ( 'NONE', *, *, #1419, .T. ) ;
#11817 = EDGE_LOOP ( 'NONE', ( #14039, #3079, #10921, #3685 ) ) ;
#11818 = AXIS2_PLACEMENT_3D ( 'NONE', #1114, #4898, #4751 ) ;
#11819 = CARTESIAN_POINT ( 'NONE',  ( 19.97461805067967688, -82.24929059928629727, -4.000000000000000888 ) ) ;
#11820 = DIRECTION ( 'NONE',  ( 0.000000000000000000, -1.000000000000000000, 0.000000000000000000 ) ) ;
#11821 = ADVANCED_FACE ( 'NONE', ( #10486 ), #6784, .T. ) ;
#11822 = AXIS2_PLACEMENT_3D ( 'NONE', #3729, #11891, #3803 ) ;
#11823 = EDGE_CURVE ( 'NONE', #7134, #2563, #5801, .T. ) ;
#11824 = PRODUCT_DEFINITION ( 'UNKNOWN', '', #189, #7047 ) ;
#11825 = CARTESIAN_POINT ( 'NONE',  ( 9.025688005465005048, -53.84505747417151156, 3.062469901903004388 ) ) ;
#11826 = CYLINDRICAL_SURFACE ( 'NONE', #3029, 4.665819364273509073 ) ;
#11827 = AXIS2_PLACEMENT_3D ( 'NONE', #11256, #7731, #11485 ) ;
#11828 = DIRECTION ( 'NONE',  ( 0.000000000000000000, 0.000000000000000000, 1.000000000000000000 ) ) ;
#11829 = ORIENTED_EDGE ( 'NONE', *, *, #12773, .F. ) ;
#11830 = MECHANICAL_DESIGN_GEOMETRIC_PRESENTATION_REPRESENTATION (  '', ( #1004 ), #14769 ) ;
#11831 = ORIENTED_EDGE ( 'NONE', *, *, #4556, .F. ) ;
#11832 = CARTESIAN_POINT ( 'NONE',  ( 64.68829635872748440, -11.56127715054218008, 76.69739539199261458 ) ) ;
#11833 = ORIENTED_EDGE ( 'NONE', *, *, #11320, .F. ) ;
#11834 = ORIENTED_EDGE ( 'NONE', *, *, #10349, .T. ) ;
#11835 = DIRECTION ( 'NONE',  ( -0.5394184268574404584, 0.8420378618367728718, 0.000000000000000000 ) ) ;
#11836 = ORIENTED_EDGE ( 'NONE', *, *, #7726, .F. ) ;
#11837 = DIRECTION ( 'NONE',  ( -0.8746197071345572782, 0.4848096202550660205, 0.000000000000000000 ) ) ;
#11838 = ORIENTED_EDGE ( 'NONE', *, *, #8061, .F. ) ;
#11839 = EDGE_CURVE ( 'NONE', #8112, #1741, #12185, .T. ) ;
#11840 = AXIS2_PLACEMENT_3D ( 'NONE', #3397, #10635, #6939 ) ;
#11841 = LINE ( 'NONE', #5781, #12444 ) ;
#11842 = CARTESIAN_POINT ( 'NONE',  ( 56.28732689558331259, 3.089731932287651084, 60.61639468829817190 ) ) ;
#11843 = ORIENTED_EDGE ( 'NONE', *, *, #9277, .T. ) ;
#11844 = AXIS2_PLACEMENT_3D ( 'NONE', #6667, #2130, #11356 ) ;
#11845 = VECTOR ( 'NONE', #1074, 1000.000000000000000 ) ;
#11846 = CARTESIAN_POINT ( 'NONE',  ( 29.35555050496136431, -52.24929059928631148, -3.199931146564432449 ) ) ;
#11847 = PLANE ( 'NONE',  #6434 ) ;
#11848 = ADVANCED_FACE ( 'NONE', ( #10334, #13719 ), #6632, .F. ) ;
#11849 = EDGE_LOOP ( 'NONE', ( #7360, #2761, #8160, #11829, #10611, #1062, #14269, #6817 ) ) ;
#11850 = LINE ( 'NONE', #11774, #6847 ) ;
#11851 = CARTESIAN_POINT ( 'NONE',  ( 52.42117158417902800, -3.175556148104785148, 48.51982618741349285 ) ) ;
#11852 = LINE ( 'NONE', #13248, #3529 ) ;
#11853 = ORIENTED_EDGE ( 'NONE', *, *, #9692, .F. ) ;
#11854 = AXIS2_PLACEMENT_3D ( 'NONE', #752, #13616, #7771 ) ;
#11855 = CARTESIAN_POINT ( 'NONE',  ( -24.72817752516938228, 2.363221963240404566, 47.50000000000012079 ) ) ;
#11856 = VECTOR ( 'NONE', #13803, 1000.000000000000000 ) ;
#11857 = AXIS2_PLACEMENT_3D ( 'NONE', #9103, #8944, #10101 ) ;
#11858 = ORIENTED_EDGE ( 'NONE', *, *, #5283, .T. ) ;
#11859 = AXIS2_PLACEMENT_3D ( 'NONE', #10996, #14313, #14529 ) ;
#11860 = DIRECTION ( 'NONE',  ( -0.000000000000000000, -0.000000000000000000, 1.000000000000000000 ) ) ;
#11861 = DIRECTION ( 'NONE',  ( 0.000000000000000000, 0.000000000000000000, 1.000000000000000000 ) ) ;
#11862 = ADVANCED_FACE ( 'NONE', ( #15182 ), #3483, .F. ) ;
#11863 = ORIENTED_EDGE ( 'NONE', *, *, #13097, .T. ) ;
#11864 = CARTESIAN_POINT ( 'NONE',  ( 8.948129010626443502, -57.91122518709997991, 2.751677560521355037 ) ) ;
#11865 = CARTESIAN_POINT ( 'NONE',  ( 23.47858629692700916, -53.24929059928630437, -6.492462156583981070 ) ) ;
#11866 = CARTESIAN_POINT ( 'NONE',  ( -16.99999999999998579, -2.249290599286303927, -58.00000000000012079 ) ) ;
#11867 = AXIS2_PLACEMENT_3D ( 'NONE', #795, #15044, #14879 ) ;
#11868 = CARTESIAN_POINT ( 'NONE',  ( 33.02192861186179584, -59.65700314074641852, -1.835602613601381883 ) ) ;
#11869 = CIRCLE ( 'NONE', #12121, 9.000000000000001776 ) ;
#11870 = CARTESIAN_POINT ( 'NONE',  ( 80.00000000000001421, -87.24929059928631148, -35.00000000000000000 ) ) ;
#11871 = CYLINDRICAL_SURFACE ( 'NONE', #703, 4.000000000000003553 ) ;
#11872 = AXIS2_PLACEMENT_3D ( 'NONE', #11306, #14776, #8703 ) ;
#11873 = EDGE_CURVE ( 'NONE', #6752, #6582, #10716, .T. ) ;
#11874 = CARTESIAN_POINT ( 'NONE',  ( 0.000000000000000000, 21.75070940071359615, 33.00000000000012790 ) ) ;
#11875 = CARTESIAN_POINT ( 'NONE',  ( 54.07385127050791596, 1.678372679529495981, 48.51982618741349285 ) ) ;
#11876 = EDGE_CURVE ( 'NONE', #7143, #6910, #3326, .T. ) ;
#11877 = ORIENTED_EDGE ( 'NONE', *, *, #5650, .F. ) ;
#11878 = PLANE ( 'NONE',  #719 ) ;
#11879 = APPLICATION_CONTEXT ( 'automotive_design' ) ;
#11880 = ORIENTED_EDGE ( 'NONE', *, *, #8882, .T. ) ;
#11881 = DIRECTION ( 'NONE',  ( 0.000000000000000000, 1.000000000000000000, -0.000000000000000000 ) ) ;
#11882 = CARTESIAN_POINT ( 'NONE',  ( 73.69809405469877106, 29.52935533987996664, 21.00807340887166674 ) ) ;
#11883 = ORIENTED_EDGE ( 'NONE', *, *, #13106, .F. ) ;
#11884 = AXIS2_PLACEMENT_3D ( 'NONE', #13290, #367, #2527 ) ;
#11885 = DIRECTION ( 'NONE',  ( 0.000000000000000000, -1.000000000000000000, -1.927470528863119788E-16 ) ) ;
#11886 = CARTESIAN_POINT ( 'NONE',  ( 105.5545870572953930, 15.25070940071369563, 139.1143251403882459 ) ) ;
#11887 = TOROIDAL_SURFACE ( 'NONE', #4006, 3.694885682588112452, 0.5000000000000000000 ) ;
#11888 = LINE ( 'NONE', #14205, #10746 ) ;
#11889 = LINE ( 'NONE', #1345, #58 ) ;
#11890 = DIRECTION ( 'NONE',  ( -0.000000000000000000, -0.000000000000000000, -1.000000000000000000 ) ) ;
#11891 = DIRECTION ( 'NONE',  ( 0.000000000000000000, 0.000000000000000000, -1.000000000000000000 ) ) ;
#11892 = DIRECTION ( 'NONE',  ( 1.000000000000000000, 0.000000000000000000, 0.000000000000000000 ) ) ;
#11893 = ORIENTED_EDGE ( 'NONE', *, *, #12483, .F. ) ;
#11894 = DIRECTION ( 'NONE',  ( -9.912705577010326782E-17, 1.000000000000000000, 1.734723475976817744E-15 ) ) ;
#11895 = EDGE_CURVE ( 'NONE', #15152, #11056, #7271, .T. ) ;
#11896 = ORIENTED_EDGE ( 'NONE', *, *, #7826, .F. ) ;
#11897 = CARTESIAN_POINT ( 'NONE',  ( 65.80512781895316721, -6.575743597179694255, 47.51982618741348574 ) ) ;
#11898 = VERTEX_POINT ( 'NONE', #7951 ) ;
#11899 = CARTESIAN_POINT ( 'NONE',  ( 64.71404714396263103, -11.54274494033589704, 76.72447063483126328 ) ) ;
#11900 = CARTESIAN_POINT ( 'NONE',  ( -16.99999999999998579, -2.249290599286303927, -50.00000000000012079 ) ) ;
#11901 = DIRECTION ( 'NONE',  ( 1.224646799147353207E-16, -1.000000000000000000, 0.000000000000000000 ) ) ;
#11902 = ORIENTED_EDGE ( 'NONE', *, *, #1913, .F. ) ;
#11903 = LINE ( 'NONE', #6066, #15070 ) ;
#11904 = LINE ( 'NONE', #6067, #1664 ) ;
#11905 = ORIENTED_EDGE ( 'NONE', *, *, #8900, .F. ) ;
#11906 = EDGE_LOOP ( 'NONE', ( #9056, #1692, #3909, #2613 ) ) ;
#11907 = EDGE_CURVE ( 'NONE', #14822, #12443, #1090, .T. ) ;
#11908 = CARTESIAN_POINT ( 'NONE',  ( 0.000000000000000000, 21.75070940071369918, 139.1143251403882459 ) ) ;
#11909 = EDGE_CURVE ( 'NONE', #10912, #6596, #7872, .T. ) ;
#11910 = ORIENTED_EDGE ( 'NONE', *, *, #4653, .T. ) ;
#11911 = CARTESIAN_POINT ( 'NONE',  ( 12.46522364980626918, -63.07964102605459544, 3.871020209143785529 ) ) ;
#11912 = ORIENTED_EDGE ( 'NONE', *, *, #12527, .F. ) ;
#11913 = DIRECTION ( 'NONE',  ( -0.000000000000000000, -0.000000000000000000, -1.000000000000000000 ) ) ;
#11914 = EDGE_LOOP ( 'NONE', ( #1489, #4123, #10956, #6570, #14624 ) ) ;
#11915 = CARTESIAN_POINT ( 'NONE',  ( -21.85476584171713199, 5.329050157244537900, -48.50000000000012079 ) ) ;
#11916 = DIRECTION ( 'NONE',  ( -0.8746197071345569451, 0.4848096202550666312, 0.000000000000000000 ) ) ;
#11917 = VERTEX_POINT ( 'NONE', #6710 ) ;
#11918 = CARTESIAN_POINT ( 'NONE',  ( 112.9262740340969060, 21.75070940071369918, 139.1143251403882459 ) ) ;
#11919 = CARTESIAN_POINT ( 'NONE',  ( -8.787473001628837821, 2.499856724289235554, 48.36782213136056896 ) ) ;
#11920 = ORIENTED_EDGE ( 'NONE', *, *, #13970, .T. ) ;
#11921 = LINE ( 'NONE', #12223, #14713 ) ;
#11922 = DIRECTION ( 'NONE',  ( -0.6727821148276317276, 0.7398406760702329610, 0.000000000000000000 ) ) ;
#11923 = CARTESIAN_POINT ( 'NONE',  ( -8.537170960192302260, 2.067018546614596719, -47.50000000000012079 ) ) ;
#11924 = ORIENTED_EDGE ( 'NONE', *, *, #6171, .F. ) ;
#11925 = ADVANCED_FACE ( 'NONE', ( #859 ), #6751, .F. ) ;
#11926 = CARTESIAN_POINT ( 'NONE',  ( 66.11195137528358146, -11.60156588980731485, 72.22102352638243872 ) ) ;
#11927 = EDGE_LOOP ( 'NONE', ( #114, #8909, #2602, #6826 ) ) ;
#11928 = ORIENTED_EDGE ( 'NONE', *, *, #7824, .T. ) ;
#11929 = CARTESIAN_POINT ( 'NONE',  ( 118.0000000000000568, 2.046973701652633381E-13, 139.1143251403882459 ) ) ;
#11930 = PRESENTATION_STYLE_ASSIGNMENT (( #7242 ) ) ;
#11931 = ORIENTED_EDGE ( 'NONE', *, *, #647, .F. ) ;
#11932 = CLOSED_SHELL ( 'NONE', ( #3897, #430, #14456, #7644, #5277, #10173, #3134, #309, #5154, #13247, #5723, #9318, #12705, #6985, #8000, #4915, #926, #7808, #9803, #12847, #2619, #7957, #8209, #843, #3584, #3545, #11100, #3814, #2689, #5678, #7849, #13940, #3492, #9314, #814, #12503, #8746, #8243, #7601, #7123, #6130, #448, #8659, #18, #10849, #7890, #4093, #13324, #1145, #10807, #3080, #1597, #12059, #10830, #9336, #7288, #4700, #1977, #9819, #6262, #5526, #4489 ) ) ;
#11933 = VERTEX_POINT ( 'NONE', #12013 ) ;
#11934 = APPLICATION_PROTOCOL_DEFINITION ( 'draft international standard', 'automotive_design', 1998, #13438 ) ;
#11935 = CARTESIAN_POINT ( 'NONE',  ( -10.31821280924931372, -8.288623256088383684, -47.74919337097148286 ) ) ;
#11936 = CARTESIAN_POINT ( 'NONE',  ( -24.96222495693456978, -7.431276100536581275, 48.50000000000012079 ) ) ;
#11937 = DIRECTION ( 'NONE',  ( -0.000000000000000000, -0.000000000000000000, 1.000000000000000000 ) ) ;
#11938 = VECTOR ( 'NONE', #13256, 1000.000000000000000 ) ;
#11939 = CARTESIAN_POINT ( 'NONE',  ( 17.93383279432583421, -62.59345883551662126, 6.358786672824582098 ) ) ;
#11940 = DIRECTION ( 'NONE',  ( -0.000000000000000000, 0.000000000000000000, 1.000000000000000000 ) ) ;
#11941 = CARTESIAN_POINT ( 'NONE',  ( 54.85055839958032209, 0.000000000000000000, 33.00000000000012790 ) ) ;
#11942 = CARTESIAN_POINT ( 'NONE',  ( 31.47353884241217159, -52.79727339576417222, 2.610417277227879307 ) ) ;
#11943 = EDGE_CURVE ( 'NONE', #14405, #1184, #25, .T. ) ;
#11944 = CARTESIAN_POINT ( 'NONE',  ( 32.39362946278320976, -53.50309148220193833, -3.187126068577873728 ) ) ;
#11945 = AXIS2_PLACEMENT_3D ( 'NONE', #14332, #889, #11506 ) ;
#11946 = DIRECTION ( 'NONE',  ( 0.000000000000000000, 0.000000000000000000, -1.000000000000000000 ) ) ;
#11947 = ORIENTED_EDGE ( 'NONE', *, *, #13889, .F. ) ;
#11948 = DIRECTION ( 'NONE',  ( 0.000000000000000000, 0.000000000000000000, 1.000000000000000000 ) ) ;
#11949 = FACE_OUTER_BOUND ( 'NONE', #10972, .T. ) ;
#11950 = CARTESIAN_POINT ( 'NONE',  ( 46.91810375148135392, 0.000000000000000000, 139.1143251403882459 ) ) ;
#11951 = DIRECTION ( 'NONE',  ( 0.9744556954135530358, 0.2245798247307374262, 0.000000000000000000 ) ) ;
#11952 = EDGE_CURVE ( 'NONE', #8699, #15028, #3639, .T. ) ;
#11953 = ADVANCED_FACE ( 'NONE', ( #9728 ), #10795, .T. ) ;
#11954 = CARTESIAN_POINT ( 'NONE',  ( 69.99380555487256572, -3.213667230009126463, 75.47065687321054384 ) ) ;
#11955 = PLANE ( 'NONE',  #9660 ) ;
#11956 = VECTOR ( 'NONE', #6664, 1000.000000000000000 ) ;
#11957 = CIRCLE ( 'NONE', #3847, 4.496540510819673209 ) ;
#11958 = DIRECTION ( 'NONE',  ( -0.000000000000000000, 0.000000000000000000, -1.000000000000000000 ) ) ;
#11959 = EDGE_CURVE ( 'NONE', #4834, #12374, #1324, .T. ) ;
#11960 = VECTOR ( 'NONE', #10439, 1000.000000000000000 ) ;
#11961 = CARTESIAN_POINT ( 'NONE',  ( 31.94053544990188342, -53.09518070810378987, 3.364836540203623549 ) ) ;
#11962 =( GEOMETRIC_REPRESENTATION_CONTEXT ( 3 ) GLOBAL_UNCERTAINTY_ASSIGNED_CONTEXT ( ( #7203 ) ) GLOBAL_UNIT_ASSIGNED_CONTEXT ( ( #14861, #12639, #6628 ) ) REPRESENTATION_CONTEXT ( 'NONE', 'WORKASPACE' ) );
#11963 = ORIENTED_EDGE ( 'NONE', *, *, #13269, .T. ) ;
#11964 = LINE ( 'NONE', #6055, #13686 ) ;
#11965 = ORIENTED_EDGE ( 'NONE', *, *, #1382, .F. ) ;
#11966 = DIRECTION ( 'NONE',  ( 1.000000000000000000, 0.000000000000000000, 0.000000000000000000 ) ) ;
#11967 = VECTOR ( 'NONE', #3186, 1000.000000000000000 ) ;
#11968 = VERTEX_POINT ( 'NONE', #4942 ) ;
#11970 = EDGE_LOOP ( 'NONE', ( #4308, #14016, #11370, #11458 ) ) ;
#11969 = CARTESIAN_POINT ( 'NONE',  ( 66.38598137497019991, -11.47113225237460377, 76.19766410831375936 ) ) ;
#11971 = DIRECTION ( 'NONE',  ( 1.000000000000000000, 0.000000000000000000, 0.000000000000000000 ) ) ;
#11972 = SHAPE_REPRESENTATION ( 'Locking Handle', ( #6315 ), #4840 ) ;
#11973 = PLANE ( 'NONE',  #9910 ) ;
#11974 = CARTESIAN_POINT ( 'NONE',  ( -16.99999999999998579, -2.249290599286305703, 33.00000000000012790 ) ) ;
#11975 = AXIS2_PLACEMENT_3D ( 'NONE', #15202, #6806, #15050 ) ;
#11976 = ADVANCED_FACE ( 'NONE', ( #1172 ), #14259, .T. ) ;
#11977 = CIRCLE ( 'NONE', #2652, 0.7892041907098256148 ) ;
#11978 = CARTESIAN_POINT ( 'NONE',  ( 20.86173033120691045, -53.24929059928630437, 0.000000000000000000 ) ) ;
#11979 = CARTESIAN_POINT ( 'NONE',  ( -16.99999999999998579, -2.249290599286303927, -58.00000000000012079 ) ) ;
#11980 = ORIENTED_EDGE ( 'NONE', *, *, #5937, .T. ) ;
#11981 = ORIENTED_EDGE ( 'NONE', *, *, #8390, .F. ) ;
#11982 = CARTESIAN_POINT ( 'NONE',  ( 52.72354942432796321, 0.2729788054883388049, 48.51982618741349285 ) ) ;
#11983 = VERTEX_POINT ( 'NONE', #14184 ) ;
#11984 = CYLINDRICAL_SURFACE ( 'NONE', #999, 0.7892041907098262810 ) ;
#11985 = VECTOR ( 'NONE', #11757, 1000.000000000000000 ) ;
#11986 = VERTEX_POINT ( 'NONE', #10569 ) ;
#11987 = CARTESIAN_POINT ( 'NONE',  ( -3.035218482312739496, 5.248692456477230373, -57.50000000000012079 ) ) ;
#11988 = ORIENTED_EDGE ( 'NONE', *, *, #2442, .T. ) ;
#11989 = AXIS2_PLACEMENT_3D ( 'NONE', #11552, #2176, #860 ) ;
#11990 = LINE ( 'NONE', #2683, #5568 ) ;
#11991 = CARTESIAN_POINT ( 'NONE',  ( 20.86173033120691045, -57.24929059928630437, 3.000000000000000888 ) ) ;
#11992 = ORIENTED_EDGE ( 'NONE', *, *, #9039, .T. ) ;
#11993 = PLANE ( 'NONE',  #6425 ) ;
#11994 = CARTESIAN_POINT ( 'NONE',  ( 80.00000000000001421, -85.24929059928629727, -8.000000000000001776 ) ) ;
#11995 = ORIENTED_EDGE ( 'NONE', *, *, #3630, .T. ) ;
#11996 = EDGE_CURVE ( 'NONE', #2589, #9131, #4714, .T. ) ;
#11997 = EDGE_CURVE ( 'NONE', #9911, #5507, #4058, .T. ) ;
#11998 = CIRCLE ( 'NONE', #12244, 0.7892041907098303888 ) ;
#11999 = DIRECTION ( 'NONE',  ( 0.000000000000000000, 0.000000000000000000, -1.000000000000000000 ) ) ;
#12000 = DIRECTION ( 'NONE',  ( -0.000000000000000000, -1.000000000000000000, -1.682156097916903736E-15 ) ) ;
#12001 = DIRECTION ( 'NONE',  ( -0.000000000000000000, 1.000000000000000000, 1.445602896647339163E-16 ) ) ;
#12002 = AXIS2_PLACEMENT_3D ( 'NONE', #11656, #8123, #126 ) ;
#12003 = ORIENTED_EDGE ( 'NONE', *, *, #11014, .F. ) ;
#12004 = FACE_OUTER_BOUND ( 'NONE', #829, .T. ) ;
#12005 = EDGE_LOOP ( 'NONE', ( #13683, #11255 ) ) ;
#12006 = CARTESIAN_POINT ( 'NONE',  ( 34.14268298385128730, 5.258265827056129993, 91.03215601016300695 ) ) ;
#12007 = CARTESIAN_POINT ( 'NONE',  ( 72.56943418881560603, -14.89867611640088896, 76.13615421477460643 ) ) ;
#12008 = VERTEX_POINT ( 'NONE', #3560 ) ;
#12009 = SHAPE_DEFINITION_REPRESENTATION ( #2041, #2630 ) ;
#12010 = DIRECTION ( 'NONE',  ( -1.000000000000000000, 0.000000000000000000, -0.000000000000000000 ) ) ;
#12011 = CARTESIAN_POINT ( 'NONE',  ( 57.26556849154462725, -7.256479411572841265, 62.84860122826521689 ) ) ;
#12012 = EDGE_CURVE ( 'NONE', #6626, #3181, #9490, .T. ) ;
#12013 = CARTESIAN_POINT ( 'NONE',  ( -65.00000000000001421, -87.24929059928631148, -17.50000000000000000 ) ) ;
#12014 = DIRECTION ( 'NONE',  ( 1.156482317317870492E-16, -1.000000000000000000, 0.000000000000000000 ) ) ;
#12015 = AXIS2_PLACEMENT_3D ( 'NONE', #9475, #160, #4850 ) ;
#12016 = CARTESIAN_POINT ( 'NONE',  ( 32.48858144966465744, -60.63355790302721715, 1.939046661991518095 ) ) ;
#12017 = PLANE ( 'NONE',  #15196 ) ;
#12018 = DIRECTION ( 'NONE',  ( 0.8746197071345560570, -0.4848096202550682410, 0.000000000000000000 ) ) ;
#12019 = CARTESIAN_POINT ( 'NONE',  ( -24.55590860040002710, -7.139109479066534369, 48.24517880332174968 ) ) ;
#12020 = CARTESIAN_POINT ( 'NONE',  ( 32.05323433862615445, -54.31204422905957330, -3.261005077968392563 ) ) ;
#12021 = VECTOR ( 'NONE', #4005, 1000.000000000000000 ) ;
#12022 = CIRCLE ( 'NONE', #14719, 0.7892041907098273912 ) ;
#12023 = LINE ( 'NONE', #1408, #14008 ) ;
#12024 = ORIENTED_EDGE ( 'NONE', *, *, #7567, .F. ) ;
#12025 = CARTESIAN_POINT ( 'NONE',  ( -80.00000000000001421, -74.24929059928631148, -4.000000000000000000 ) ) ;
#12026 = CARTESIAN_POINT ( 'NONE',  ( 33.12442989620986822, -59.21224831720011395, 2.500000000000000000 ) ) ;
#12027 = DIRECTION ( 'NONE',  ( 0.8208219420614810691, -0.4549890321264228876, -0.3453061251629915285 ) ) ;
#12028 = LINE ( 'NONE', #14124, #7306 ) ;
#12029 = CARTESIAN_POINT ( 'NONE',  ( 69.36169026123523906, -3.800370218431805114, 77.14753538332058724 ) ) ;
#12030 = PLANE ( 'NONE',  #7668 ) ;
#12031 = TOROIDAL_SURFACE ( 'NONE', #8593, 3.694885682587998765, 0.5000000000000000000 ) ;
#12032 = AXIS2_PLACEMENT_3D ( 'NONE', #9500, #11946, #11721 ) ;
#12033 = B_SPLINE_CURVE_WITH_KNOTS ( 'NONE', 3,
 ( #2961, #4101, #493, #1507, #14438, #356 ),
 .UNSPECIFIED., .F., .F.,
 ( 4, 2, 4 ),
 ( 0.000000000000000000, 0.0003908577252344191651, 0.0007817154504688383302 ),
 .UNSPECIFIED. ) ;
#12034 = EDGE_CURVE ( 'NONE', #9345, #7966, #13031, .T. ) ;
#12035 = CARTESIAN_POINT ( 'NONE',  ( 64.79680489028815771, -11.48253646253152560, 71.59064503457959461 ) ) ;
#12036 = LINE ( 'NONE', #8644, #11070 ) ;
#12037 = CARTESIAN_POINT ( 'NONE',  ( -16.99999999999998579, -2.249290599286303927, -47.50000000000012079 ) ) ;
#12038 = CARTESIAN_POINT ( 'NONE',  ( 57.51704887355756313, 3.283153786997079049, 48.51982618741349285 ) ) ;
#12039 = EDGE_CURVE ( 'NONE', #7398, #2221, #6051, .T. ) ;
#12040 = ORIENTED_EDGE ( 'NONE', *, *, #4744, .T. ) ;
#12041 = EDGE_CURVE ( 'NONE', #13017, #4396, #14695, .T. ) ;
#12042 = DIRECTION ( 'NONE',  ( 0.000000000000000000, 0.000000000000000000, 1.000000000000000000 ) ) ;
#12043 = ORIENTED_EDGE ( 'NONE', *, *, #10223, .F. ) ;
#12044 = CARTESIAN_POINT ( 'NONE',  ( 15.46081644285383483, -69.39711819508849544, -5.076148092048929250 ) ) ;
#12045 = CIRCLE ( 'NONE', #7139, 4.999999999999997335 ) ;
#12046 = ORIENTED_EDGE ( 'NONE', *, *, #2458, .T. ) ;
#12047 = ORIENTED_EDGE ( 'NONE', *, *, #9149, .T. ) ;
#12049 = VERTEX_POINT ( 'NONE', #14482 ) ;
#12048 = CARTESIAN_POINT ( 'NONE',  ( -11.83418063572647760, -2.249290599286303927, 58.00000000000012079 ) ) ;
#12050 = DIRECTION ( 'NONE',  ( -0.8746197071345571672, 0.4848096202550659650, 0.000000000000000000 ) ) ;
#12051 = EDGE_CURVE ( 'NONE', #13513, #7624, #13541, .T. ) ;
#12052 = DIRECTION ( 'NONE',  ( -1.000000000000000000, 0.000000000000000000, 0.000000000000000000 ) ) ;
#12053 = ORIENTED_EDGE ( 'NONE', *, *, #2967, .F. ) ;
#12054 = CARTESIAN_POINT ( 'NONE',  ( -30.80945343098651890, -5.389243620311580329, 58.00000000000012079 ) ) ;
#12055 = VECTOR ( 'NONE', #7569, 1000.000000000000000 ) ;
#12056 = EDGE_CURVE ( 'NONE', #6921, #3262, #5165, .T. ) ;
#12057 = CARTESIAN_POINT ( 'NONE',  ( 80.18290120114222930, 25.52935533987996664, 33.00000000000012790 ) ) ;
#12058 = CARTESIAN_POINT ( 'NONE',  ( 20.86173033120691045, -72.24929059928631148, 3.999999999999999112 ) ) ;
#12059 = ADVANCED_FACE ( 'NONE', ( #11019 ), #11080, .F. ) ;
#12060 = ORIENTED_EDGE ( 'NONE', *, *, #6369, .F. ) ;
#12061 = ORIENTED_EDGE ( 'NONE', *, *, #165, .F. ) ;
#12062 = EDGE_CURVE ( 'NONE', #3816, #10484, #10085, .T. ) ;
#12063 = CARTESIAN_POINT ( 'NONE',  ( 58.00000000000000711, -2.249290599286309256, 47.51982618741348574 ) ) ;
#12064 = ORIENTED_EDGE ( 'NONE', *, *, #1792, .T. ) ;
#12065 = ORIENTED_EDGE ( 'NONE', *, *, #11562, .F. ) ;
#12066 =( BOUNDED_SURFACE ( )  B_SPLINE_SURFACE ( 3, 2, ( 
 ( #10965, #3447, #3530 ),
 ( #415, #5115, #14503 ),
 ( #7648, #5414, #705 ),
 ( #1798, #7800, #2956 ),
 ( #11109, #11251, #5499 ),
 ( #11034, #1939, #12342 ),
 ( #4249, #2870, #13407 ),
 ( #12493, #5336, #6636 ),
 ( #10033, #14795, #10187 ),
 ( #4020, #4322, #6490 ) ),
 .UNSPECIFIED., .F., .F., .F. ) 
 B_SPLINE_SURFACE_WITH_KNOTS ( ( 4, 2, 2, 2, 4 ),
 ( 3, 3 ),
 ( 0.0006711510808134562266, 0.001062132081067026709, 0.001453113081320597409, 0.001844094081574168108, 0.002235075081827738591 ),
 ( 0.000000000000000000, 1.000000000000000000 ),
 .UNSPECIFIED. ) 
 GEOMETRIC_REPRESENTATION_ITEM ( )  RATIONAL_B_SPLINE_SURFACE ( (
 ( 1.000000000000000000, 0.7254762501099963901, 1.000000000000000000),
 ( 1.000000000000000000, 0.7255094664176422459, 1.000000000000000000),
 ( 1.000000000000000000, 0.7239949553644952074, 1.000000000000000000),
 ( 1.000000000000000000, 0.7190573720639429345, 1.000000000000000000),
 ( 1.000000000000000000, 0.7156412189950915881, 1.000000000000000000),
 ( 1.000000000000000000, 0.7094102539594338008, 1.000000000000000000),
 ( 1.000000000000000000, 0.7066203625162998936, 1.000000000000000000),
 ( 1.000000000000000000, 0.7042417591947802702, 1.000000000000000000),
 ( 1.000000000000000000, 0.7046402682201203804, 1.000000000000000000),
 ( 1.000000000000000000, 0.7071067811865500152, 1.000000000000000000) ) ) 
 REPRESENTATION_ITEM ( '' )  SURFACE ( )  );
#12067 = CARTESIAN_POINT ( 'NONE',  ( -22.54958699671023581, 4.838095916862976686, 48.21133583021728697 ) ) ;
#12068 = ORIENTED_EDGE ( 'NONE', *, *, #2886, .T. ) ;
#12069 = CARTESIAN_POINT ( 'NONE',  ( 14.09856246968322147, -52.24929059928629727, 4.899481419391097603 ) ) ;
#12070 = AXIS2_PLACEMENT_3D ( 'NONE', #2274, #4341, #11415 ) ;
#12071 = EDGE_CURVE ( 'NONE', #9229, #1375, #4649, .T. ) ;
#12072 = EDGE_LOOP ( 'NONE', ( #11524, #12837, #1323, #13377 ) ) ;
#12073 = DIRECTION ( 'NONE',  ( -1.000000000000000000, -0.000000000000000000, -0.000000000000000000 ) ) ;
#12074 = CARTESIAN_POINT ( 'NONE',  ( -11.86108202630535224, -9.639858853941328576, 48.38337049880509255 ) ) ;
#12075 = ORIENTED_EDGE ( 'NONE', *, *, #8610, .F. ) ;
#12076 = CARTESIAN_POINT ( 'NONE',  ( 28.56975842969204038, -65.65107448351471930, -3.408697305255637300 ) ) ;
#12077 = VECTOR ( 'NONE', #14914, 1000.000000000000000 ) ;
#12078 = ORIENTED_EDGE ( 'NONE', *, *, #5025, .F. ) ;
#12079 = AXIS2_PLACEMENT_3D ( 'NONE', #938, #4487, #5890 ) ;
#12080 = CIRCLE ( 'NONE', #5692, 0.5000000000000004441 ) ;
#12081 = CARTESIAN_POINT ( 'NONE',  ( 58.00000000000000711, -2.249290599286309256, 82.40005259842790508 ) ) ;
#12082 = CYLINDRICAL_SURFACE ( 'NONE', #3715, 0.5000000000000004441 ) ;
#12083 = CARTESIAN_POINT ( 'NONE',  ( 104.9938193859979236, 0.000000000000000000, 33.00000000000012790 ) ) ;
#12084 = ORIENTED_EDGE ( 'NONE', *, *, #395, .T. ) ;
#12085 = LINE ( 'NONE', #1468, #11493 ) ;
#12086 = ORIENTED_EDGE ( 'NONE', *, *, #14180, .T. ) ;
#12087 = VECTOR ( 'NONE', #3718, 1000.000000000000000 ) ;
#12088 = EDGE_CURVE ( 'NONE', #153, #7206, #6764, .T. ) ;
#12089 = ORIENTED_EDGE ( 'NONE', *, *, #8499, .T. ) ;
#12090 = AXIS2_PLACEMENT_3D ( 'NONE', #635, #7732, #2878 ) ;
#12091 = ADVANCED_FACE ( 'NONE', ( #1842 ), #5242, .F. ) ;
#12092 = CARTESIAN_POINT ( 'NONE',  ( -3.190546569013415379, 0.8906624217387615339, -48.00000000000012079 ) ) ;
#12093 = ORIENTED_EDGE ( 'NONE', *, *, #5326, .T. ) ;
#12094 = AXIS2_PLACEMENT_3D ( 'NONE', #7195, #4889, #9592 ) ;
#12095 = APPLICATION_PROTOCOL_DEFINITION ( 'draft international standard', 'automotive_design', 1998, #14340 ) ;
#12096 = DIRECTION ( 'NONE',  ( 0.8746197071345571672, -0.4848096202550661316, 0.000000000000000000 ) ) ;
#12097 = DIRECTION ( 'NONE',  ( -1.000000000000000000, 0.000000000000000000, 0.000000000000000000 ) ) ;
#12098 = CARTESIAN_POINT ( 'NONE',  ( -11.05444845021228595, -9.014367880605227867, -48.04486892757390848 ) ) ;
#12099 = VERTEX_POINT ( 'NONE', #6534 ) ;
#12100 = FACE_OUTER_BOUND ( 'NONE', #4911, .T. ) ;
#12101 = TOROIDAL_SURFACE ( 'NONE', #3237, 8.500000000000000000, 0.5000000000000000000 ) ;
#12102 = DIRECTION ( 'NONE',  ( -0.000000000000000000, 0.000000000000000000, -1.000000000000000000 ) ) ;
#12103 = AXIS2_PLACEMENT_3D ( 'NONE', #11293, #9159, #748 ) ;
#12104 = CARTESIAN_POINT ( 'NONE',  ( -2.016677571526633510E-15, 23.25070940071368497, -33.00000000000012790 ) ) ;
#12105 = CARTESIAN_POINT ( 'NONE',  ( 32.21801100873970114, -53.34475964609211474, -2.389227176380471551 ) ) ;
#12106 = VECTOR ( 'NONE', #12166, 1000.000000000000000 ) ;
#12107 = EDGE_CURVE ( 'NONE', #6772, #750, #8698, .T. ) ;
#12108 = CARTESIAN_POINT ( 'NONE',  ( 112.9262740340969060, 23.25070940071369563, 33.00000000000012790 ) ) ;
#12109 = EDGE_CURVE ( 'NONE', #4512, #9348, #5093, .T. ) ;
#12110 = ORIENTED_EDGE ( 'NONE', *, *, #6340, .T. ) ;
#12111 = DIRECTION ( 'NONE',  ( -0.000000000000000000, 0.000000000000000000, -1.000000000000000000 ) ) ;
#12112 = CARTESIAN_POINT ( 'NONE',  ( 32.77533165179128360, -57.91122518710081124, -2.751677560519801169 ) ) ;
#12113 = VECTOR ( 'NONE', #714, 1000.000000000000000 ) ;
#12114 = DIRECTION ( 'NONE',  ( 1.000000000000000000, 0.000000000000000000, 0.000000000000000000 ) ) ;
#12115 = CARTESIAN_POINT ( 'NONE',  ( 69.43180921594577626, -3.262091255642812992, 75.98418538769692532 ) ) ;
#12116 = DIRECTION ( 'NONE',  ( -1.000000000000000000, 0.000000000000000000, 0.000000000000000000 ) ) ;
#12117 = VECTOR ( 'NONE', #8457, 1000.000000000000000 ) ;
#12118 = DIRECTION ( 'NONE',  ( 0.000000000000000000, -0.000000000000000000, -1.000000000000000000 ) ) ;
#12119 = CYLINDRICAL_SURFACE ( 'NONE', #3227, 3.999999999999999112 ) ;
#12120 = ORIENTED_EDGE ( 'NONE', *, *, #8626, .T. ) ;
#12121 = AXIS2_PLACEMENT_3D ( 'NONE', #10302, #7611, #6453 ) ;
#12122 = CARTESIAN_POINT ( 'NONE',  ( 33.74207955331441156, -53.52407281596779143, -2.732083154000400693 ) ) ;
#12123 = PRODUCT_DEFINITION_CONTEXT ( 'detailed design', #14340, 'design' ) ;
#12124 = CIRCLE ( 'NONE', #12620, 0.5000000000000003331 ) ;
#12125 = ORIENTED_EDGE ( 'NONE', *, *, #11499, .F. ) ;
#12126 = LINE ( 'NONE', #1583, #291 ) ;
#12127 = DIRECTION ( 'NONE',  ( 0.000000000000000000, -1.000000000000000000, 0.000000000000000000 ) ) ;
#12128 = VERTEX_POINT ( 'NONE', #2785 ) ;
#12129 = ORIENTED_EDGE ( 'NONE', *, *, #10614, .T. ) ;
#12130 = DIRECTION ( 'NONE',  ( -0.000000000000000000, -0.000000000000000000, -1.000000000000000000 ) ) ;
#12131 = LINE ( 'NONE', #62, #4336 ) ;
#12132 = DIRECTION ( 'NONE',  ( -0.8746197071345572782, 0.4848096202550659650, 0.000000000000000000 ) ) ;
#12133 = ORIENTED_EDGE ( 'NONE', *, *, #11025, .T. ) ;
#12134 = CARTESIAN_POINT ( 'NONE',  ( 9.047572573828887244, -55.23312247377393192, 2.984220967394216828 ) ) ;
#12135 = VECTOR ( 'NONE', #517, 1000.000000000000000 ) ;
#12136 = EDGE_CURVE ( 'NONE', #6074, #9111, #12425, .T. ) ;
#12137 = CARTESIAN_POINT ( 'NONE',  ( 21.74884261173415467, -82.24929059928629727, -4.000000000000000888 ) ) ;
#12138 = LINE ( 'NONE', #12429, #3387 ) ;
#12139 = ADVANCED_FACE ( 'NONE', ( #6392 ), #7765, .F. ) ;
#12140 = VERTEX_POINT ( 'NONE', #7481 ) ;
#12141 = VERTEX_POINT ( 'NONE', #682 ) ;
#12142 = CARTESIAN_POINT ( 'NONE',  ( 54.85055839958032209, 0.000000000000000000, -33.00000000000012790 ) ) ;
#12143 = ORIENTED_EDGE ( 'NONE', *, *, #12758, .T. ) ;
#12144 = ORIENTED_EDGE ( 'NONE', *, *, #12527, .T. ) ;
#12145 = FACE_OUTER_BOUND ( 'NONE', #14466, .T. ) ;
#12146 = ORIENTED_EDGE ( 'NONE', *, *, #6687, .T. ) ;
#12147 = CARTESIAN_POINT ( 'NONE',  ( 25.53229935574759679, -53.25924492462442572, 5.664691252382116460 ) ) ;
#12148 = ORIENTED_EDGE ( 'NONE', *, *, #5371, .F. ) ;
#12149 = DIRECTION ( 'NONE',  ( 8.673617379884035472E-17, -1.000000000000000000, 0.000000000000000000 ) ) ;
#12150 = DIRECTION ( 'NONE',  ( 0.000000000000000000, -0.000000000000000000, -1.000000000000000000 ) ) ;
#12151 = ORIENTED_EDGE ( 'NONE', *, *, #11473, .F. ) ;
#12152 = EDGE_CURVE ( 'NONE', #2314, #6609, #9799, .T. ) ;
#12153 = EDGE_CURVE ( 'NONE', #11311, #3243, #8342, .T. ) ;
#12154 = CARTESIAN_POINT ( 'NONE',  ( 27.79575038568401268, -66.12098470289947727, -4.407543342774902229 ) ) ;
#12155 = VERTEX_POINT ( 'NONE', #10394 ) ;
#12156 = CARTESIAN_POINT ( 'NONE',  ( -28.95977857253363297, -8.587818791446675704, 48.50000000000012079 ) ) ;
#12157 = DIRECTION ( 'NONE',  ( -0.000000000000000000, -0.000000000000000000, 1.000000000000000000 ) ) ;
#12158 = DIRECTION ( 'NONE',  ( -0.000000000000000000, -0.000000000000000000, -1.000000000000000000 ) ) ;
#12159 = VERTEX_POINT ( 'NONE', #6760 ) ;
#12160 = CARTESIAN_POINT ( 'NONE',  ( 61.57781019154727176, -5.828480965243416634, 60.61639468829817190 ) ) ;
#12161 = VERTEX_POINT ( 'NONE', #12465 ) ;
#12162 = ORIENTED_EDGE ( 'NONE', *, *, #8304, .T. ) ;
#12163 = DIRECTION ( 'NONE',  ( 0.000000000000000000, 0.000000000000000000, -1.000000000000000000 ) ) ;
#12164 = PRODUCT_CONTEXT ( 'NONE', #2443, 'mechanical' ) ;
#12165 = LINE ( 'NONE', #6183, #665 ) ;
#12166 = DIRECTION ( 'NONE',  ( 0.000000000000000000, 0.000000000000000000, 1.000000000000000000 ) ) ;
#12167 = DIRECTION ( 'NONE',  ( 0.000000000000000000, -0.000000000000000000, -1.000000000000000000 ) ) ;
#12168 = CARTESIAN_POINT ( 'NONE',  ( 13.56565975558667247, -63.36830850588443553, 4.156137255536471287 ) ) ;
#12169 = B_SPLINE_CURVE_WITH_KNOTS ( 'NONE', 3,
 ( #11846, #14239, #4776, #7085 ),
 .UNSPECIFIED., .F., .F.,
 ( 4, 4 ),
 ( 0.000000000000000000, 0.006683255761480911238 ),
 .UNSPECIFIED. ) ;
#12170 = DIRECTION ( 'NONE',  ( 1.000000000000000000, 0.000000000000000000, 0.000000000000000000 ) ) ;
#12171 = EDGE_CURVE ( 'NONE', #14067, #9700, #3155, .T. ) ;
#12172 = CARTESIAN_POINT ( 'NONE',  ( 33.63127143586577716, -56.35534736560776992, 1.852150208425979105 ) ) ;
#12173 = CARTESIAN_POINT ( 'NONE',  ( 13.86797143582181491, -68.67521603617278458, -4.260811380361852585 ) ) ;
#12174 = CARTESIAN_POINT ( 'NONE',  ( 27.33382790127958728, -69.39711819508849544, 4.502057496415716287 ) ) ;
#12175 = ORIENTED_EDGE ( 'NONE', *, *, #3730, .T. ) ;
#12176 = DIRECTION ( 'NONE',  ( 0.000000000000000000, -0.000000000000000000, -1.000000000000000000 ) ) ;
#12177 = DIRECTION ( 'NONE',  ( 1.000000000000000000, -0.000000000000000000, 0.000000000000000000 ) ) ;
#12178 = CARTESIAN_POINT ( 'NONE',  ( 0.9298897195970434737, -1.451567674087680837, 48.50000000000012079 ) ) ;
#12179 = DIRECTION ( 'NONE',  ( 1.000000000000000000, 0.000000000000000000, 0.000000000000000000 ) ) ;
#12180 = CARTESIAN_POINT ( 'NONE',  ( 11.08747240253766897, -53.42215338339673281, 3.801984355195809240 ) ) ;
#12181 = DIRECTION ( 'NONE',  ( 0.9421718071228325497, 2.933300018044979975E-16, 0.3351302520855077294 ) ) ;
#12182 = CARTESIAN_POINT ( 'NONE',  ( 54.85055839958032209, 23.25070940071368852, 33.00000000000012790 ) ) ;
#12183 = EDGE_CURVE ( 'NONE', #11054, #4463, #13657, .T. ) ;
#12184 = CARTESIAN_POINT ( 'NONE',  ( 8.597635011448856446, -59.20619211347771937, -2.502190571104460748 ) ) ;
#12185 = CIRCLE ( 'NONE', #1626, 3.694885682587998765 ) ;
#12186 = ORIENTED_EDGE ( 'NONE', *, *, #9582, .T. ) ;
#12187 = CARTESIAN_POINT ( 'NONE',  ( 29.14641708242553619, -50.05591495609735375, -4.211963358982893091 ) ) ;
#12188 = ORIENTED_EDGE ( 'NONE', *, *, #11010, .T. ) ;
#12189 = CARTESIAN_POINT ( 'NONE',  ( -21.16581936427349575, -2.249290599286303483, 50.00000000000012079 ) ) ;
#12190 = CARTESIAN_POINT ( 'NONE',  ( 58.00000000000000711, -2.249290599286309256, 38.50000000000012790 ) ) ;
#12191 = ORIENTED_EDGE ( 'NONE', *, *, #11606, .F. ) ;
#12192 = DIRECTION ( 'NONE',  ( -1.000000000000000000, 0.000000000000000000, 0.000000000000000000 ) ) ;
#12193 = CARTESIAN_POINT ( 'NONE',  ( -16.99999999999998579, -2.249290599286303927, 48.00000000000012079 ) ) ;
#12194 = VECTOR ( 'NONE', #12677, 1000.000000000000000 ) ;
#12195 = VECTOR ( 'NONE', #13904, 1000.000000000000000 ) ;
#12196 = CARTESIAN_POINT ( 'NONE',  ( 71.80003071982790175, -14.47218880931180962, 73.19766410831374515 ) ) ;
#12197 = EDGE_CURVE ( 'NONE', #14796, #10461, #5706, .T. ) ;
#12198 = EDGE_LOOP ( 'NONE', ( #6999, #8971, #7896, #6879 ) ) ;
#12199 = FACE_OUTER_BOUND ( 'NONE', #12613, .T. ) ;
#12200 = AXIS2_PLACEMENT_3D ( 'NONE', #1191, #4886, #12972 ) ;
#12201 = DIRECTION ( 'NONE',  ( 1.000000000000000000, 0.000000000000000000, -0.000000000000000000 ) ) ;
#12202 = PLANE ( 'NONE',  #4355 ) ;
#12203 = AXIS2_PLACEMENT_3D ( 'NONE', #3942, #5409, #5179 ) ;
#12204 = VERTEX_POINT ( 'NONE', #1917 ) ;
#12205 = ORIENTED_EDGE ( 'NONE', *, *, #13830, .T. ) ;
#12206 = CIRCLE ( 'NONE', #10245, 11.46463184759104870 ) ;
#12207 = FACE_BOUND ( 'NONE', #7152, .T. ) ;
#12208 = EDGE_LOOP ( 'NONE', ( #6382, #4510 ) ) ;
#12209 = CARTESIAN_POINT ( 'NONE',  ( 14.39660873059139767, -68.54636829475870741, 4.542647641079955001 ) ) ;
#12210 = ORIENTED_EDGE ( 'NONE', *, *, #8455, .T. ) ;
#12211 = CYLINDRICAL_SURFACE ( 'NONE', #10822, 0.5000000000000000000 ) ;
#12212 = ADVANCED_FACE ( 'NONE', ( #3384, #10312 ), #11379, .T. ) ;
#12213 = AXIS2_PLACEMENT_3D ( 'NONE', #12928, #2220, #15080 ) ;
#12214 = VERTEX_POINT ( 'NONE', #12625 ) ;
#12215 = PRODUCT_DEFINITION_FORMATION_WITH_SPECIFIED_SOURCE ( 'ANY', '', #10155, .NOT_KNOWN. ) ;
#12216 = FACE_OUTER_BOUND ( 'NONE', #13511, .T. ) ;
#12217 = CARTESIAN_POINT ( 'NONE',  ( -25.46282903980766932, -6.565599745187317815, 57.50000000000012079 ) ) ;
#12218 = ORIENTED_EDGE ( 'NONE', *, *, #7971, .T. ) ;
#12219 = CIRCLE ( 'NONE', #2875, 6.000000000000000000 ) ;
#12220 = DIRECTION ( 'NONE',  ( -0.000000000000000000, -0.000000000000000000, 1.000000000000000000 ) ) ;
#12221 = CIRCLE ( 'NONE', #11475, 6.484807146443463566 ) ;
#12222 = VERTEX_POINT ( 'NONE', #6614 ) ;
#12223 = CARTESIAN_POINT ( 'NONE',  ( 58.00000000000000711, 23.25070940071368852, 139.1143251403882459 ) ) ;
#12224 = CARTESIAN_POINT ( 'NONE',  ( -80.00000000000001421, -76.24929059928631148, 6.000000000000000000 ) ) ;
#12225 = EDGE_CURVE ( 'NONE', #8468, #7944, #12696, .T. ) ;
#12226 = CARTESIAN_POINT ( 'NONE',  ( 109.8334623555409735, 23.25070940071369563, 139.1143251403882459 ) ) ;
#12227 = VECTOR ( 'NONE', #13365, 1000.000000000000000 ) ;
#12228 = ORIENTED_EDGE ( 'NONE', *, *, #3730, .F. ) ;
#12229 = CARTESIAN_POINT ( 'NONE',  ( 114.0000000000000284, 15.25070940071369563, 33.00000000000012790 ) ) ;
#12230 = EDGE_CURVE ( 'NONE', #8078, #2314, #7855, .T. ) ;
#12231 = ORIENTED_EDGE ( 'NONE', *, *, #6143, .F. ) ;
#12232 = TOROIDAL_SURFACE ( 'NONE', #5604, 10.46463184759104870, 1.000000000000000000 ) ;
#12233 = ORIENTED_EDGE ( 'NONE', *, *, #7272, .T. ) ;
#12234 = EDGE_CURVE ( 'NONE', #12856, #8652, #759, .T. ) ;
#12235 = CIRCLE ( 'NONE', #5606, 0.9999999999999954481 ) ;
#12236 = EDGE_CURVE ( 'NONE', #9304, #12214, #11528, .T. ) ;
#12237 =( REPRESENTATION_RELATIONSHIP ('NONE','NONE', #15125, #3114 ) REPRESENTATION_RELATIONSHIP_WITH_TRANSFORMATION ( #6322 )SHAPE_REPRESENTATION_RELATIONSHIP( ) );
#12238 = ORIENTED_EDGE ( 'NONE', *, *, #2256, .T. ) ;
#12239 = CARTESIAN_POINT ( 'NONE',  ( 19.97461805067967688, -82.24929059928629727, -6.000000000000000888 ) ) ;
#12240 = PRODUCT_CONTEXT ( 'NONE', #14245, 'mechanical' ) ;
#12241 = DIRECTION ( 'NONE',  ( -0.000000000000000000, -0.000000000000000000, -1.000000000000000000 ) ) ;
#12242 = CARTESIAN_POINT ( 'NONE',  ( 80.18290120114222930, 23.25070940071369208, 33.00000000000012790 ) ) ;
#12243 = EDGE_CURVE ( 'NONE', #1375, #9911, #4538, .T. ) ;
#12244 = AXIS2_PLACEMENT_3D ( 'NONE', #13478, #12554, #4304 ) ;
#12245 = CARTESIAN_POINT ( 'NONE',  ( 8.821484763567294607, -57.33450387999030795, -2.749014434309871469 ) ) ;
#12246 = ORIENTED_EDGE ( 'NONE', *, *, #1236, .T. ) ;
#12247 = CARTESIAN_POINT ( 'NONE',  ( 17.53865101127114201, -70.79589105106622071, 6.161139702144408758 ) ) ;
#12248 = VECTOR ( 'NONE', #5903, 1000.000000000000000 ) ;
#12249 = CARTESIAN_POINT ( 'NONE',  ( 33.07363029493502182, -59.43266865480772765, 1.834006918418328524 ) ) ;
#12250 = LINE ( 'NONE', #7627, #14978 ) ;
#12251 = DIRECTION ( 'NONE',  ( 1.000000000000000000, 0.000000000000000000, 0.000000000000000000 ) ) ;
#12252 = FACE_OUTER_BOUND ( 'NONE', #2023, .T. ) ;
#12253 = ADVANCED_FACE ( 'NONE', ( #11616 ), #769, .T. ) ;
#12254 = ORIENTED_EDGE ( 'NONE', *, *, #6154, .T. ) ;
#12255 = CARTESIAN_POINT ( 'NONE',  ( 33.52366768382369600, -57.47994873761392398, -2.501453769636603486 ) ) ;
#12256 = FACE_OUTER_BOUND ( 'NONE', #8459, .T. ) ;
#12257 = ORIENTED_EDGE ( 'NONE', *, *, #5611, .T. ) ;
#12258 = EDGE_CURVE ( 'NONE', #11609, #9619, #1073, .T. ) ;
#12259 = CARTESIAN_POINT ( 'NONE',  ( 8.741728328725566044, -56.83124152802056983, 2.758380730586871277 ) ) ;
#12260 =( NAMED_UNIT ( * ) PLANE_ANGLE_UNIT ( ) SI_UNIT ( $, .RADIAN. ) );
#12261 = DIRECTION ( 'NONE',  ( 9.912705577010325549E-17, -1.734723475976817547E-15, 1.000000000000000000 ) ) ;
#12262 = DIRECTION ( 'NONE',  ( 0.000000000000000000, 0.000000000000000000, 1.000000000000000000 ) ) ;
#12263 = AXIS2_PLACEMENT_3D ( 'NONE', #6846, #3159, #10014 ) ;
#12264 = CARTESIAN_POINT ( 'NONE',  ( 30.60592481596645342, -62.41236107492795782, -2.580051240451693317 ) ) ;
#12265 = VERTEX_POINT ( 'NONE', #6691 ) ;
#12266 = CARTESIAN_POINT ( 'NONE',  ( 24.01697609495870367, -67.68160391992793734, -6.249260988559870000 ) ) ;
#12267 = ORIENTED_EDGE ( 'NONE', *, *, #2430, .F. ) ;
#12268 = CARTESIAN_POINT ( 'NONE',  ( 62.14930354033766946, 1.441842398587370067, 60.61639468829817190 ) ) ;
#12269 = LINE ( 'NONE', #1724, #4735 ) ;
#12270 = VERTEX_POINT ( 'NONE', #9082 ) ;
#12272 = ORIENTED_EDGE ( 'NONE', *, *, #5899, .F. ) ;
#12271 = DIRECTION ( 'NONE',  ( -0.000000000000000000, -0.000000000000000000, -1.000000000000000000 ) ) ;
#12273 = DIRECTION ( 'NONE',  ( -9.912705577010326536E-16, 0.000000000000000000, 1.000000000000000000 ) ) ;
#12274 = EDGE_CURVE ( 'NONE', #7187, #8918, #11584, .T. ) ;
#12275 = EDGE_CURVE ( 'NONE', #11141, #5016, #8925, .T. ) ;
#12276 = AXIS2_PLACEMENT_3D ( 'NONE', #5497, #12646, #13956 ) ;
#12277 = CARTESIAN_POINT ( 'NONE',  ( 11.84453356674751845, -63.30956378474061808, 2.875213255991846406 ) ) ;
#12278 = CARTESIAN_POINT ( 'NONE',  ( 12.05519880765550411, -52.24929059928630437, 3.114712537286230098 ) ) ;
#12279 = FACE_OUTER_BOUND ( 'NONE', #8596, .T. ) ;
#12280 = CARTESIAN_POINT ( 'NONE',  ( -24.90998783373886738, 2.881753107372537759, -48.00000000000012079 ) ) ;
#12281 = ORIENTED_EDGE ( 'NONE', *, *, #9241, .T. ) ;
#12282 = VERTEX_POINT ( 'NONE', #14088 ) ;
#12283 = CARTESIAN_POINT ( 'NONE',  ( 9.276103490588601730, -60.71989949371947404, 2.646748467230720436 ) ) ;
#12284 = ORIENTED_EDGE ( 'NONE', *, *, #3452, .F. ) ;
#12285 = CARTESIAN_POINT ( 'NONE',  ( 14.38963276113423895, -69.39711819508849544, 4.502057496415707405 ) ) ;
#12286 = ORIENTED_EDGE ( 'NONE', *, *, #6273, .T. ) ;
#12287 = FACE_OUTER_BOUND ( 'NONE', #13435, .T. ) ;
#12288 = EDGE_CURVE ( 'NONE', #7044, #3003, #522, .T. ) ;
#12289 = EDGE_CURVE ( 'NONE', #3921, #6752, #6016, .T. ) ;
#12290 = DIRECTION ( 'NONE',  ( 0.000000000000000000, 0.000000000000000000, 1.000000000000000000 ) ) ;
#12291 = EDGE_CURVE ( 'NONE', #15191, #2378, #12169, .T. ) ;
#12292 = PRODUCT_DEFINITION ( 'UNKNOWN', '', #12215, #3517 ) ;
#12293 = CARTESIAN_POINT ( 'NONE',  ( 54.21883389619742388, -5.612936290787406968, 60.61639468829817190 ) ) ;
#12294 = DIRECTION ( 'NONE',  ( 0.8656763553492640151, 0.5006040828730974335, 0.000000000000000000 ) ) ;
#12295 = VERTEX_POINT ( 'NONE', #3614 ) ;
#12296 = AXIS2_PLACEMENT_3D ( 'NONE', #693, #10325, #7866 ) ;
#12297 = CARTESIAN_POINT ( 'NONE',  ( 31.12893072307018016, -61.89517205449885751, -2.369674354392826920 ) ) ;
#12298 = ORIENTED_EDGE ( 'NONE', *, *, #12275, .T. ) ;
#12299 = CARTESIAN_POINT ( 'NONE',  ( 23.10474973039555380, -52.24929059928630437, 5.564967562786275579 ) ) ;
#12300 = DIRECTION ( 'NONE',  ( 1.000000000000000000, 0.000000000000000000, 0.000000000000000000 ) ) ;
#12301 = CARTESIAN_POINT ( 'NONE',  ( 53.11142512232702018, -3.558169932106523881, 60.61639468829817190 ) ) ;
#12302 = DIRECTION ( 'NONE',  ( 0.000000000000000000, 1.734723475976817547E-15, -1.000000000000000000 ) ) ;
#12303 = ORIENTED_EDGE ( 'NONE', *, *, #13970, .F. ) ;
#12304 = AXIS2_PLACEMENT_3D ( 'NONE', #6272, #1499, #9888 ) ;
#12305 = CARTESIAN_POINT ( 'NONE',  ( -12.14523415828296216, -9.827631355817223024, -48.00000000000012079 ) ) ;
#12306 = ORIENTED_EDGE ( 'NONE', *, *, #2754, .F. ) ;
#12307 = VERTEX_POINT ( 'NONE', #3542 ) ;
#12308 = ORIENTED_EDGE ( 'NONE', *, *, #3608, .F. ) ;
#12309 = CARTESIAN_POINT ( 'NONE',  ( 80.00000000000001421, -85.24929059928629727, -8.000000000000001776 ) ) ;
#12310 = AXIS2_PLACEMENT_3D ( 'NONE', #8132, #3736, #15211 ) ;
#12311 = CARTESIAN_POINT ( 'NONE',  ( 58.00000000000000711, -2.249290599286311032, 38.00000000000012079 ) ) ;
#12312 = EDGE_CURVE ( 'NONE', #3688, #9584, #10850, .T. ) ;
#12313 = CYLINDRICAL_SURFACE ( 'NONE', #10632, 0.7892041907098262810 ) ;
#12314 = CARTESIAN_POINT ( 'NONE',  ( 60.65595175199513278, -6.557103238384438981, 48.51982618741349285 ) ) ;
#12315 = CIRCLE ( 'NONE', #14771, 4.194885682588113340 ) ;
#12316 = VERTEX_POINT ( 'NONE', #9471 ) ;
#12317 = ORIENTED_EDGE ( 'NONE', *, *, #13641, .F. ) ;
#12318 = DIRECTION ( 'NONE',  ( 0.000000000000000000, 1.000000000000000000, -0.000000000000000000 ) ) ;
#12319 = CARTESIAN_POINT ( 'NONE',  ( 65.88530916257730041, -11.69141299361105979, 72.29513642469299839 ) ) ;
#12320 = DIRECTION ( 'NONE',  ( -0.9876883405935777960, 0.1564344650500800460, 0.000000000000000000 ) ) ;
#12321 = DIRECTION ( 'NONE',  ( -0.000000000000000000, 0.000000000000000000, -1.000000000000000000 ) ) ;
#12322 = CARTESIAN_POINT ( 'NONE',  ( 47.27423575335444639, 25.52935533987996664, 84.20452624982236500 ) ) ;
#12323 = VERTEX_POINT ( 'NONE', #4925 ) ;
#12324 = AXIS2_PLACEMENT_3D ( 'NONE', #4586, #3520, #8221 ) ;
#12325 = PLANE ( 'NONE',  #4122 ) ;
#12326 = VECTOR ( 'NONE', #1684, 1000.000000000000000 ) ;
#12327 = EDGE_CURVE ( 'NONE', #5697, #1905, #235, .T. ) ;
#12328 = AXIS2_PLACEMENT_3D ( 'NONE', #4171, #7877, #13567 ) ;
#12329 = CARTESIAN_POINT ( 'NONE',  ( -2.016677571526633510E-15, 23.25070940071368497, 33.00000000000012790 ) ) ;
#12330 = ORIENTED_EDGE ( 'NONE', *, *, #8518, .F. ) ;
#12331 = CARTESIAN_POINT ( 'NONE',  ( 8.091875466796945915, -56.84639887601247921, -1.823510762986219058 ) ) ;
#12332 = CARTESIAN_POINT ( 'NONE',  ( -12.41494337171168283, -9.406612424898836977, 58.00000000000012079 ) ) ;
#12333 = ORIENTED_EDGE ( 'NONE', *, *, #7345, .F. ) ;
#12334 = DIRECTION ( 'NONE',  ( 1.000000000000000000, 0.000000000000000000, 0.000000000000000000 ) ) ;
#12335 =( GEOMETRIC_REPRESENTATION_CONTEXT ( 3 ) GLOBAL_UNCERTAINTY_ASSIGNED_CONTEXT ( ( #14435 ) ) GLOBAL_UNIT_ASSIGNED_CONTEXT ( ( #2945, #6546, #11392 ) ) REPRESENTATION_CONTEXT ( 'NONE', 'WORKASPACE' ) );
#12336 = AXIS2_PLACEMENT_3D ( 'NONE', #4804, #8276, #4957 ) ;
#12337 = ADVANCED_FACE ( 'NONE', ( #4846, #4692 ), #9395, .F. ) ;
#12338 = VECTOR ( 'NONE', #3692, 1000.000000000000000 ) ;
#12339 = EDGE_CURVE ( 'NONE', #8234, #8955, #10548, .T. ) ;
#12340 = CARTESIAN_POINT ( 'NONE',  ( -20.99999999999998579, -67.96969602390581144, 33.00000000000001421 ) ) ;
#12341 = FACE_OUTER_BOUND ( 'NONE', #5779, .T. ) ;
#12342 = CARTESIAN_POINT ( 'NONE',  ( -24.73660316015754290, -6.848489080522048411, -47.70033363922482295 ) ) ;
#12343 = ORIENTED_EDGE ( 'NONE', *, *, #13654, .T. ) ;
#12344 = CARTESIAN_POINT ( 'NONE',  ( -12.99999999999998757, -2.249290599286301706, -115.4621125123531442 ) ) ;
#12345 = TOROIDAL_SURFACE ( 'NONE', #3215, 1.000000000000000000, 0.5000000000000000000 ) ;
#12346 = ORIENTED_EDGE ( 'NONE', *, *, #12275, .F. ) ;
#12347 = CARTESIAN_POINT ( 'NONE',  ( 29.69047892279256473, -53.28399145779480506, -4.141535524925036960 ) ) ;
#12348 = LINE ( 'NONE', #7504, #15046 ) ;
#12349 = CIRCLE ( 'NONE', #7683, 2.499999999999995115 ) ;
#12350 = ORIENTED_EDGE ( 'NONE', *, *, #4537, .T. ) ;
#12351 = FACE_OUTER_BOUND ( 'NONE', #7167, .T. ) ;
#12352 = CARTESIAN_POINT ( 'NONE',  ( 45.17127246049422240, 23.25070940071368852, -33.00000000000012790 ) ) ;
#12353 = VECTOR ( 'NONE', #4756, 1000.000000000000000 ) ;
#12354 = ORIENTED_EDGE ( 'NONE', *, *, #13197, .T. ) ;
#12355 = CARTESIAN_POINT ( 'NONE',  ( 10.45251858057167915, -61.76394201828934882, 3.065891788195822976 ) ) ;
#12356 = AXIS2_PLACEMENT_3D ( 'NONE', #13968, #15198, #4651 ) ;
#12357 = DIRECTION ( 'NONE',  ( -0.000000000000000000, 0.000000000000000000, -1.000000000000000000 ) ) ;
#12358 = VECTOR ( 'NONE', #6829, 1000.000000000000000 ) ;
#12359 = DIRECTION ( 'NONE',  ( 1.000000000000000000, 0.000000000000000000, 0.000000000000000000 ) ) ;
#12360 = EDGE_CURVE ( 'NONE', #3217, #8760, #3691, .T. ) ;
#12361 = CARTESIAN_POINT ( 'NONE',  ( 80.00000000000001421, -72.24929059928631148, -32.99999999999999289 ) ) ;
#12362 = VECTOR ( 'NONE', #10073, 1000.000000000000000 ) ;
#12363 = ORIENTED_EDGE ( 'NONE', *, *, #12731, .T. ) ;
#12364 = LINE ( 'NONE', #8895, #14656 ) ;
#12365 = EDGE_CURVE ( 'NONE', #1600, #5032, #7661, .T. ) ;
#12366 = VERTEX_POINT ( 'NONE', #4618 ) ;
#12367 = CARTESIAN_POINT ( 'NONE',  ( 120.4255624041552721, -41.42576115427227990, 51.74171249506144932 ) ) ;
#12368 = ORIENTED_EDGE ( 'NONE', *, *, #6154, .F. ) ;
#12369 = CARTESIAN_POINT ( 'NONE',  ( -29.99999999999998224, -69.24929059928631148, -115.4621125123531442 ) ) ;
#12370 = LINE ( 'NONE', #13169, #12687 ) ;
#12371 = AXIS2_PLACEMENT_3D ( 'NONE', #11498, #3579, #5824 ) ;
#12372 = DIRECTION ( 'NONE',  ( 0.000000000000000000, -0.000000000000000000, 1.000000000000000000 ) ) ;
#12373 = DIRECTION ( 'NONE',  ( 0.000000000000000000, 0.000000000000000000, -1.000000000000000000 ) ) ;
#12374 = VERTEX_POINT ( 'NONE', #14163 ) ;
#12375 = DIRECTION ( 'NONE',  ( 0.000000000000000000, 0.000000000000000000, -1.000000000000000000 ) ) ;
#12376 = ORIENTED_EDGE ( 'NONE', *, *, #9720, .T. ) ;
#12377 = DIRECTION ( 'NONE',  ( -1.000000000000000000, 0.000000000000000000, 0.000000000000000000 ) ) ;
#12378 = DIRECTION ( 'NONE',  ( 8.659560562354330119E-17, 0.7071067811865966446, -0.7071067811864982788 ) ) ;
#12379 = EDGE_CURVE ( 'NONE', #65, #4729, #8394, .T. ) ;
#12380 = EDGE_CURVE ( 'NONE', #14796, #13684, #7231, .T. ) ;
#12381 = LINE ( 'NONE', #4210, #7465 ) ;
#12382 = VERTEX_POINT ( 'NONE', #9630 ) ;
#12383 = DIRECTION ( 'NONE',  ( 0.000000000000000000, 0.000000000000000000, 1.000000000000000000 ) ) ;
#12384 = ORIENTED_EDGE ( 'NONE', *, *, #13851, .T. ) ;
#12385 = EDGE_LOOP ( 'NONE', ( #9702, #6255, #12734, #4314 ) ) ;
#12386 = ORIENTED_EDGE ( 'NONE', *, *, #7582, .F. ) ;
#12387 = DIRECTION ( 'NONE',  ( -0.000000000000000000, -1.000000000000000000, -0.000000000000000000 ) ) ;
#12388 = B_SPLINE_CURVE_WITH_KNOTS ( 'NONE', 3,
 ( #8485, #13385, #6100, #7542, #2622, #6319, #7318, #11013 ),
 .UNSPECIFIED., .F., .F.,
 ( 4, 2, 2, 4 ),
 ( 8.673617379884035472E-19, 0.0006709104321108796693, 0.001341820864221758471, 0.002683641728443498728 ),
 .UNSPECIFIED. ) ;
#12389 = DIRECTION ( 'NONE',  ( 1.000000000000000000, 0.000000000000000000, 0.000000000000000000 ) ) ;
#12390 = FACE_BOUND ( 'NONE', #14696, .T. ) ;
#12391 = CARTESIAN_POINT ( 'NONE',  ( -16.99999999999998579, -2.249290599286303927, -38.00000000000012079 ) ) ;
#12392 = EDGE_LOOP ( 'NONE', ( #3393, #281, #650, #4291, #7591 ) ) ;
#12393 = EDGE_CURVE ( 'NONE', #3816, #12099, #1016, .T. ) ;
#12394 = DIRECTION ( 'NONE',  ( 1.000000000000000000, 0.000000000000000000, 0.000000000000000000 ) ) ;
#12395 = CARTESIAN_POINT ( 'NONE',  ( 65.71319926014257362, -10.73129157630437724, 71.19766410831374515 ) ) ;
#12396 = DIRECTION ( 'NONE',  ( 1.734723475976807292E-15, -1.000000000000000000, 0.000000000000000000 ) ) ;
#12397 = FACE_OUTER_BOUND ( 'NONE', #4150, .T. ) ;
#12398 = CARTESIAN_POINT ( 'NONE',  ( 10.59452993935777165, -61.89517205451002013, -2.369674354332441446 ) ) ;
#12399 = ORIENTED_EDGE ( 'NONE', *, *, #222, .F. ) ;
#12400 = CARTESIAN_POINT ( 'NONE',  ( 95.31453344691183815, 0.000000000000000000, 139.1143251403882459 ) ) ;
#12401 = DIRECTION ( 'NONE',  ( 0.8656763553493062036, 0.5006040828730242698, 0.000000000000000000 ) ) ;
#12402 = ORIENTED_EDGE ( 'NONE', *, *, #5099, .F. ) ;
#12403 = DIRECTION ( 'NONE',  ( 1.000000000000000000, 0.000000000000000000, 0.000000000000000000 ) ) ;
#12404 = CARTESIAN_POINT ( 'NONE',  ( 47.97280705105441001, 3.308873213108443512, 82.40005259842790508 ) ) ;
#12405 = DIRECTION ( 'NONE',  ( -0.000000000000000000, 0.000000000000000000, 1.000000000000000000 ) ) ;
#12406 = VERTEX_POINT ( 'NONE', #7305 ) ;
#12407 = CARTESIAN_POINT ( 'NONE',  ( 112.9262740340969060, 23.25070940071369563, -13.14990448602692474 ) ) ;
#12408 = ADVANCED_FACE ( 'NONE', ( #1228 ), #11993, .F. ) ;
#12409 = DIRECTION ( 'NONE',  ( 0.000000000000000000, 0.000000000000000000, 1.000000000000000000 ) ) ;
#12410 = PLANE ( 'NONE',  #6858 ) ;
#12411 = DIRECTION ( 'NONE',  ( -0.8746197071345569451, 0.4848096202550666312, 0.000000000000000000 ) ) ;
#12412 = EDGE_LOOP ( 'NONE', ( #9862, #15193, #12900, #11269, #6160, #6158, #12936, #9900, #14194 ) ) ;
#12413 = PLANE ( 'NONE',  #14730 ) ;
#12414 = ORIENTED_EDGE ( 'NONE', *, *, #1328, .T. ) ;
#12415 = EDGE_CURVE ( 'NONE', #12323, #7276, #2312, .T. ) ;
#12416 = CARTESIAN_POINT ( 'NONE',  ( 27.62489819270789582, -52.24929059928629727, -4.899481419331793042 ) ) ;
#12417 = CARTESIAN_POINT ( 'NONE',  ( 59.59091026602544616, -7.053490217115945704, 62.84860122826521689 ) ) ;
#12418 = EDGE_CURVE ( 'NONE', #2170, #14421, #5865, .T. ) ;
#12419 = ORIENTED_EDGE ( 'NONE', *, *, #4469, .T. ) ;
#12420 = CARTESIAN_POINT ( 'NONE',  ( 82.49066175147797253, 12.46743062497963450, 84.20452624982236500 ) ) ;
#12421 = DIRECTION ( 'NONE',  ( -0.8420378618367728718, -0.5394184268574404584, 0.000000000000000000 ) ) ;
#12422 = ORIENTED_EDGE ( 'NONE', *, *, #5470, .T. ) ;
#12423 = CARTESIAN_POINT ( 'NONE',  ( 13.49335920019251134, -64.93526722763070325, 4.251815205945346676 ) ) ;
#12424 = EDGE_CURVE ( 'NONE', #404, #14080, #87, .T. ) ;
#12425 = CIRCLE ( 'NONE', #5810, 8.500000000000000000 ) ;
#12426 = DIRECTION ( 'NONE',  ( -0.000000000000000000, 1.000000000000000000, 1.445602896647339163E-16 ) ) ;
#12427 = FACE_OUTER_BOUND ( 'NONE', #1429, .T. ) ;
#12428 = EDGE_CURVE ( 'NONE', #11668, #10777, #1522, .T. ) ;
#12429 = CARTESIAN_POINT ( 'NONE',  ( 84.72310019870096198, 29.52935533987996664, -33.00000000000013500 ) ) ;
#12430 = ORIENTED_EDGE ( 'NONE', *, *, #1872, .T. ) ;
#12431 = CARTESIAN_POINT ( 'NONE',  ( 9.976190356295422390, -60.51242536180875931, 2.958269724473149065 ) ) ;
#12432 = ORIENTED_EDGE ( 'NONE', *, *, #2468, .F. ) ;
#12433 = CARTESIAN_POINT ( 'NONE',  ( 32.82061086202445921, -55.58404325705457438, -2.908775817946459785 ) ) ;
#12434 = ORIENTED_EDGE ( 'NONE', *, *, #580, .T. ) ;
#12435 = LINE ( 'NONE', #1889, #5920 ) ;
#12436 = AXIS2_PLACEMENT_3D ( 'NONE', #1163, #10480, #9482 ) ;
#12437 = CARTESIAN_POINT ( 'NONE',  ( -16.99999999999998579, -2.249290599286303927, 33.00000000000012790 ) ) ;
#12438 = DIRECTION ( 'NONE',  ( -0.3020115420618161295, 0.1674077314120152038, -0.9384901064608655030 ) ) ;
#12439 = PLANE ( 'NONE',  #1327 ) ;
#12440 = ORIENTED_EDGE ( 'NONE', *, *, #13013, .F. ) ;
#12441 = EDGE_CURVE ( 'NONE', #14421, #10741, #1827, .T. ) ;
#12442 = LINE ( 'NONE', #6745, #12833 ) ;
#12443 = VERTEX_POINT ( 'NONE', #13241 ) ;
#12444 = VECTOR ( 'NONE', #4690, 1000.000000000000000 ) ;
#12445 = AXIS2_PLACEMENT_3D ( 'NONE', #9902, #14582, #8881 ) ;
#12446 = CARTESIAN_POINT ( 'NONE',  ( 80.00000000000001421, -72.24929059928631148, 32.99999999999999289 ) ) ;
#12447 = CARTESIAN_POINT ( 'NONE',  ( 114.6731053250840233, 21.75070940071369918, 13.14990448602693007 ) ) ;
#12448 = DIRECTION ( 'NONE',  ( 0.000000000000000000, 0.000000000000000000, 1.000000000000000000 ) ) ;
#12449 = DIRECTION ( 'NONE',  ( 0.000000000000000000, 0.000000000000000000, 1.000000000000000000 ) ) ;
#12450 = ORIENTED_EDGE ( 'NONE', *, *, #10388, .T. ) ;
#12451 = DIRECTION ( 'NONE',  ( 1.000000000000000000, 0.000000000000000000, 0.000000000000000000 ) ) ;
#12452 = VECTOR ( 'NONE', #5926, 1000.000000000000000 ) ;
#12453 = ORIENTED_EDGE ( 'NONE', *, *, #12197, .T. ) ;
#12454 = FACE_OUTER_BOUND ( 'NONE', #3336, .T. ) ;
#12455 = AXIS2_PLACEMENT_3D ( 'NONE', #2647, #7418, #407 ) ;
#12456 = VERTEX_POINT ( 'NONE', #9990 ) ;
#12457 = ORIENTED_EDGE ( 'NONE', *, *, #12757, .F. ) ;
#12458 = CARTESIAN_POINT ( 'NONE',  ( 27.76589651684735927, -69.39711819508849544, 4.056575093033438328 ) ) ;
#12459 = AXIS2_PLACEMENT_3D ( 'NONE', #9590, #2578, #8356 ) ;
#12460 = DIRECTION ( 'NONE',  ( 1.000000000000000000, 0.000000000000000000, 0.000000000000000000 ) ) ;
#12461 = PLANE ( 'NONE',  #4231 ) ;
#12462 = ADVANCED_FACE ( 'NONE', ( #14676 ), #10932, .T. ) ;
#12463 = EDGE_CURVE ( 'NONE', #10969, #13205, #4130, .T. ) ;
#12464 =( BOUNDED_SURFACE ( )  B_SPLINE_SURFACE ( 3, 2, ( 
 ( #6296, #14306, #13153 ),
 ( #9547, #13298, #374 ),
 ( #3757, #14386, #1532 ),
 ( #6237, #3827, #13234 ),
 ( #8469, #2605, #2681 ),
 ( #5067, #13078, #14461 ),
 ( #14525, #3905, #8601 ),
 ( #2760, #10991, #447 ),
 ( #6010, #5140, #2456 ),
 ( #10693, #4837, #11057 ),
 ( #13436, #11351, #1964 ),
 ( #5524, #6662, #3058 ),
 ( #6440, #14596, #6511 ),
 ( #512, #11273, #10211 ) ),
 .UNSPECIFIED., .F., .F., .F. ) 
 B_SPLINE_SURFACE_WITH_KNOTS ( ( 4, 2, 2, 2, 2, 2, 4 ),
 ( 3, 3 ),
 ( 0.000000000000000000, 0.002560658414910374665, 0.003840987622365561998, 0.005121316829820749331, 0.006401646037275936230, 0.007681975244731123996, 0.01024263365964149866 ),
 ( 0.000000000000000000, 1.000000000000000000 ),
 .UNSPECIFIED. ) 
 GEOMETRIC_REPRESENTATION_ITEM ( )  RATIONAL_B_SPLINE_SURFACE ( (
 ( 1.000000000000000000, 0.8053615646146035090, 1.000000000000000000),
 ( 1.000000000000000000, 0.8105996499491424645, 1.000000000000000000),
 ( 1.000000000000000000, 0.8160199193853241439, 1.000000000000000000),
 ( 1.000000000000000000, 0.8240376314735337049, 1.000000000000000000),
 ( 1.000000000000000000, 0.8266971106454457097, 1.000000000000000000),
 ( 1.000000000000000000, 0.8319110421178486092, 1.000000000000000000),
 ( 1.000000000000000000, 0.8344214672177644454, 1.000000000000000000),
 ( 1.000000000000000000, 0.8392107060239341054, 1.000000000000000000),
 ( 1.000000000000000000, 0.8414897010531580124, 1.000000000000000000),
 ( 1.000000000000000000, 0.8457750297010538931, 1.000000000000000000),
 ( 1.000000000000000000, 0.8477871175333944187, 1.000000000000000000),
 ( 1.000000000000000000, 0.8533050377659684438, 1.000000000000000000),
 ( 1.000000000000000000, 0.8561733496717280900, 1.000000000000000000),
 ( 1.000000000000000000, 0.8581891718822901582, 1.000000000000000000) ) ) 
 REPRESENTATION_ITEM ( '' )  SURFACE ( )  );
#12465 = CARTESIAN_POINT ( 'NONE',  ( -32.80254285330622821, -2.278009980413885582, 58.00000000000012079 ) ) ;
#12466 = VERTEX_POINT ( 'NONE', #7528 ) ;
#12467 = AXIS2_PLACEMENT_3D ( 'NONE', #1957, #6654, #805 ) ;
#12468 = ORIENTED_EDGE ( 'NONE', *, *, #9435, .T. ) ;
#12469 = CARTESIAN_POINT ( 'NONE',  ( 64.36032056549935021, -11.78815919431190196, 72.16553326196626017 ) ) ;
#12470 = CARTESIAN_POINT ( 'NONE',  ( 33.62917719264643068, -56.86702399164118304, -2.513921072345373542 ) ) ;
#12471 = VECTOR ( 'NONE', #5709, 1000.000000000000000 ) ;
#12472 = FACE_OUTER_BOUND ( 'NONE', #11037, .T. ) ;
#12473 = CARTESIAN_POINT ( 'NONE',  ( 13.13160920566000023, -64.18054652438912910, -4.118450070759328341 ) ) ;
#12474 = VERTEX_POINT ( 'NONE', #1750 ) ;
#12475 = AXIS2_PLACEMENT_3D ( 'NONE', #3402, #4241, #12562 ) ;
#12476 = CARTESIAN_POINT ( 'NONE',  ( 32.97619012053721121, -56.45473609427280337, 2.788978005137584315 ) ) ;
#12477 = DIRECTION ( 'NONE',  ( 0.000000000000000000, 0.000000000000000000, 1.000000000000000000 ) ) ;
#12478 = EDGE_LOOP ( 'NONE', ( #6365, #9168, #5574, #12802 ) ) ;
#12479 = CARTESIAN_POINT ( 'NONE',  ( 93.56770215592470663, 23.25070940071369208, 33.00000000000012790 ) ) ;
#12480 = CARTESIAN_POINT ( 'NONE',  ( 0.000000000000000000, 2.750709400713692965, 139.1143251403882459 ) ) ;
#12481 = AXIS2_PLACEMENT_3D ( 'NONE', #13382, #9933, #6459 ) ;
#12482 = ADVANCED_FACE ( 'NONE', ( #13524 ), #6206, .T. ) ;
#12483 = EDGE_CURVE ( 'NONE', #4443, #791, #379, .T. ) ;
#12484 = SHAPE_REPRESENTATION_RELATIONSHIP ( 'NONE' , 'NONE' ,  #13539, #11073 ) ;
#12485 = CARTESIAN_POINT ( 'NONE',  ( -3.999999999999976019, -72.24929059928631148, -32.99999999999999289 ) ) ;
#12486 = CARTESIAN_POINT ( 'NONE',  ( 19.97461805067967333, -85.24929059928631148, 6.000000000000001776 ) ) ;
#12487 = EDGE_LOOP ( 'NONE', ( #1943, #2678, #1740, #10602 ) ) ;
#12488 = PRODUCT_DEFINITION_SHAPE ( 'NONE', 'NONE',  #12292 ) ;
#12489 = AXIS2_PLACEMENT_3D ( 'NONE', #2196, #11414, #10354 ) ;
#12490 = LINE ( 'NONE', #8638, #7030 ) ;
#12491 = CARTESIAN_POINT ( 'NONE',  ( 29.93210037042245375, -53.28557117198399595, 4.055532625545659187 ) ) ;
#12492 = DIRECTION ( 'NONE',  ( 0.000000000000000000, 0.000000000000000000, 1.000000000000000000 ) ) ;
#12493 = CARTESIAN_POINT ( 'NONE',  ( -25.40673215887140657, -6.684475985750503391, -48.01308457333527002 ) ) ;
#12494 = ORIENTED_EDGE ( 'NONE', *, *, #7619, .T. ) ;
#12495 = CARTESIAN_POINT ( 'NONE',  ( 32.44676321640788075, -60.72048491829421124, 2.646952986714198097 ) ) ;
#12496 = ORIENTED_EDGE ( 'NONE', *, *, #1335, .F. ) ;
#12497 = PLANE ( 'NONE',  #13068 ) ;
#12498 = DIRECTION ( 'NONE',  ( 0.8746197071345590546, -0.4848096202550629674, 0.000000000000000000 ) ) ;
#12499 = ORIENTED_EDGE ( 'NONE', *, *, #5199, .T. ) ;
#12500 = CARTESIAN_POINT ( 'NONE',  ( 20.86173033120691045, -53.24929059928630437, 7.000000000000000000 ) ) ;
#12501 = DIRECTION ( 'NONE',  ( -1.000000000000000000, 0.000000000000000000, 0.000000000000000000 ) ) ;
#12502 = CARTESIAN_POINT ( 'NONE',  ( 13.65275068252399571, -65.32322779889722142, 4.310009693575397982 ) ) ;
#12503 = ADVANCED_FACE ( 'NONE', ( #11063 ), #8349, .T. ) ;
#12504 = CARTESIAN_POINT ( 'NONE',  ( 10.83536516265427352, -52.51002131803453210, 3.753497227305226946 ) ) ;
#12505 = CARTESIAN_POINT ( 'NONE',  ( 31.73919081233200856, -60.50127194134182673, 2.962969586007845102 ) ) ;
#12506 = DIRECTION ( 'NONE',  ( 1.000000000000000000, 0.000000000000000000, 0.000000000000000000 ) ) ;
#12507 = ADVANCED_FACE ( 'NONE', ( #14832 ), #7835, .F. ) ;
#12508 = ADVANCED_FACE ( 'NONE', ( #13832, #12525 ), #1970, .T. ) ;
#12509 = CARTESIAN_POINT ( 'NONE',  ( 18.00000000000001066, 0.000000000000000000, 33.00000000000012790 ) ) ;
#12510 = CARTESIAN_POINT ( 'NONE',  ( 62.67308791069655882, 29.52935533987996664, 33.00000000000014211 ) ) ;
#12511 = ORIENTED_EDGE ( 'NONE', *, *, #10450, .T. ) ;
#12512 = CARTESIAN_POINT ( 'NONE',  ( 17.78537369493905373, -66.03679020173537140, -6.288305159854754578 ) ) ;
#12513 = ORIENTED_EDGE ( 'NONE', *, *, #6666, .T. ) ;
#12514 = CIRCLE ( 'NONE', #4902, 0.5000000000000004441 ) ;
#12515 = ADVANCED_FACE ( 'NONE', ( #819 ), #7911, .T. ) ;
#12516 = CARTESIAN_POINT ( 'NONE',  ( 31.50598280721104416, -53.84004999663768132, -3.478067438360130215 ) ) ;
#12517 = CIRCLE ( 'NONE', #8818, 0.7892041907098322762 ) ;
#12518 = EDGE_LOOP ( 'NONE', ( #12917, #3064, #4989, #4446 ) ) ;
#12519 = CARTESIAN_POINT ( 'NONE',  ( 1.004339113574583608, 0.8906624217387615339, -57.50000000000012079 ) ) ;
#12520 = ADVANCED_FACE ( 'NONE', ( #3063 ), #4278, .F. ) ;
#12521 = CARTESIAN_POINT ( 'NONE',  ( -9.456839514482961562, 2.659958822950722723, 58.00000000000012079 ) ) ;
#12522 = DIRECTION ( 'NONE',  ( -0.000000000000000000, 0.000000000000000000, -1.000000000000000000 ) ) ;
#12523 = CARTESIAN_POINT ( 'NONE',  ( 12.36791015745245836, -52.24929059928631148, 2.500000000000000000 ) ) ;
#12524 = EDGE_CURVE ( 'NONE', #8767, #8156, #10065, .T. ) ;
#12525 = FACE_OUTER_BOUND ( 'NONE', #10531, .T. ) ;
#12526 = ORIENTED_EDGE ( 'NONE', *, *, #14267, .F. ) ;
#12527 = EDGE_CURVE ( 'NONE', #12265, #6058, #5703, .T. ) ;
#12528 = VECTOR ( 'NONE', #11646, 1000.000000000000114 ) ;
#12529 = EDGE_CURVE ( 'NONE', #10265, #7295, #13069, .T. ) ;
#12530 = DIRECTION ( 'NONE',  ( 1.000000000000000000, 0.000000000000000000, 0.000000000000000000 ) ) ;
#12531 = CARTESIAN_POINT ( 'NONE',  ( 8.766501742169731770, -57.08411837894907848, -2.747858231244113991 ) ) ;
#12532 = CARTESIAN_POINT ( 'NONE',  ( -7.499999999999985789, -2.249290599286303927, 48.00000000000012079 ) ) ;
#12533 = CARTESIAN_POINT ( 'NONE',  ( 109.8334623555409735, 0.000000000000000000, -33.00000000000012790 ) ) ;
#12534 = ORIENTED_EDGE ( 'NONE', *, *, #6487, .F. ) ;
#12535 = ORIENTED_EDGE ( 'NONE', *, *, #8570, .F. ) ;
#12536 = DIRECTION ( 'NONE',  ( -0.000000000000000000, -0.000000000000000000, -1.000000000000000000 ) ) ;
#12537 = ORIENTED_EDGE ( 'NONE', *, *, #5525, .F. ) ;
#12538 = FACE_OUTER_BOUND ( 'NONE', #11230, .T. ) ;
#12539 = ORIENTED_EDGE ( 'NONE', *, *, #7486, .T. ) ;
#12540 = ORIENTED_EDGE ( 'NONE', *, *, #8934, .F. ) ;
#12541 = DIRECTION ( 'NONE',  ( 0.000000000000000000, 0.000000000000000000, 1.000000000000000000 ) ) ;
#12542 = ITEM_DEFINED_TRANSFORMATION ( 'NONE', 'NONE', #14657,  #6315 ) ;
#12543 = CARTESIAN_POINT ( 'NONE',  ( 9.974161267552085874, -60.51083307721924598, -2.957531760941039423 ) ) ;
#12544 = CARTESIAN_POINT ( 'NONE',  ( 31.72322230991231962, -61.42570632716525125, 2.132522520905362651 ) ) ;
#12545 = CARTESIAN_POINT ( 'NONE',  ( 112.9262740340969060, 23.25070940071369563, 139.1143251403882459 ) ) ;
#12546 = CARTESIAN_POINT ( 'NONE',  ( -1.197457146693716057, -2.220571218158943427, -48.00000000000012079 ) ) ;
#12547 = ORIENTED_EDGE ( 'NONE', *, *, #7999, .T. ) ;
#12548 = FACE_BOUND ( 'NONE', #7979, .T. ) ;
#12549 = FACE_OUTER_BOUND ( 'NONE', #450, .T. ) ;
#12550 = CARTESIAN_POINT ( 'NONE',  ( 118.0000000000000568, 2.046973701652633381E-13, 139.1143251403882459 ) ) ;
#12551 = LINE ( 'NONE', #14558, #1046 ) ;
#12552 = CARTESIAN_POINT ( 'NONE',  ( 31.88039071915910583, -62.60658208069056485, 2.715520055361023477 ) ) ;
#12553 = ORIENTED_EDGE ( 'NONE', *, *, #4142, .F. ) ;
#12554 = DIRECTION ( 'NONE',  ( 0.000000000000000000, 0.000000000000000000, 1.000000000000000000 ) ) ;
#12555 = EDGE_CURVE ( 'NONE', #12474, #11368, #15033, .T. ) ;
#12556 = CARTESIAN_POINT ( 'NONE',  ( 58.00000000000000711, 0.000000000000000000, -33.00000000000012790 ) ) ;
#12557 = EDGE_LOOP ( 'NONE', ( #4277, #9397, #9980, #13158 ) ) ;
#12558 =( BOUNDED_SURFACE ( )  B_SPLINE_SURFACE ( 3, 2, ( 
 ( #5907, #3804, #9677 ),
 ( #14364, #7199, #12983 ),
 ( #7273, #2658, #14281 ),
 ( #4745, #3731, #129 ),
 ( #11659, #8443, #6053 ),
 ( #9360, #12908, #4968 ),
 ( #10517, #11961, #10739 ),
 ( #15206, #9442, #4815 ),
 ( #276, #4662, #14133 ),
 ( #14053, #10669, #9515 ),
 ( #1201, #201, #13129 ),
 ( #8214, #2432, #1424 ),
 ( #6129, #2583, #8286 ),
 ( #13053, #3580, #2351 ),
 ( #14210, #7043, #10816 ),
 ( #11740, #10589, #7127 ),
 ( #3663, #11810, #1270 ),
 ( #5984, #4892, #5482 ),
 ( #6479, #13551, #1780 ),
 ( #7864, #6699, #4157 ),
 ( #12476, #10094, #3019 ),
 ( #7712, #617, #5322 ),
 ( #9951, #14938, #6210 ),
 ( #768, #4393, #10020 ) ),
 .UNSPECIFIED., .F., .F., .F. ) 
 B_SPLINE_SURFACE_WITH_KNOTS ( ( 4, 2, 2, 2, 2, 2, 2, 2, 2, 2, 2, 4 ),
 ( 3, 3 ),
 ( 0.000000000000000000, 0.0007569831467696884432, 0.001513966293539376886, 0.002270949440309065221, 0.002649441013693909497, 0.003027932587078753773, 0.003406424160463598048, 0.003784915733848441891, 0.004541898880618130442, 0.004920390454002974284, 0.005298882027387818994, 0.006055865174157507545 ),
 ( 0.000000000000000000, 1.000000000000000000 ),
 .UNSPECIFIED. ) 
 GEOMETRIC_REPRESENTATION_ITEM ( )  RATIONAL_B_SPLINE_SURFACE ( (
 ( 1.000000000000000000, 0.6947298545087511323, 1.000000000000000000),
 ( 1.000000000000000000, 0.7030359819960161349, 1.000000000000000000),
 ( 1.000000000000000000, 0.7110141033721932846, 1.000000000000000000),
 ( 1.000000000000000000, 0.7265357204475346720, 1.000000000000000000),
 ( 1.000000000000000000, 0.7341632328267053698, 1.000000000000000000),
 ( 1.000000000000000000, 0.7486333683864616617, 1.000000000000000000),
 ( 1.000000000000000000, 0.7555062062380646370, 1.000000000000000000),
 ( 1.000000000000000000, 0.7654404118662447853, 1.000000000000000000),
 ( 1.000000000000000000, 0.7687038416331641866, 1.000000000000000000),
 ( 1.000000000000000000, 0.7749762558335999696, 1.000000000000000000),
 ( 1.000000000000000000, 0.7780012814123101750, 1.000000000000000000),
 ( 1.000000000000000000, 0.7838538191794924836, 1.000000000000000000),
 ( 1.000000000000000000, 0.7866813202764355584, 1.000000000000000000),
 ( 1.000000000000000000, 0.7921509987295953792, 1.000000000000000000),
 ( 1.000000000000000000, 0.7948100380742536553, 1.000000000000000000),
 ( 1.000000000000000000, 0.8023666703953391544, 1.000000000000000000),
 ( 1.000000000000000000, 0.8068432255863590141, 1.000000000000000000),
 ( 1.000000000000000000, 0.8126963150101803590, 1.000000000000000000),
 ( 1.000000000000000000, 0.8145123882373950241, 1.000000000000000000),
 ( 1.000000000000000000, 0.8177588193891505153, 1.000000000000000000),
 ( 1.000000000000000000, 0.8191832667250861233, 1.000000000000000000),
 ( 1.000000000000000000, 0.8228396104941044786, 1.000000000000000000),
 ( 1.000000000000000000, 0.8244610879124180114, 1.000000000000000000),
 ( 1.000000000000000000, 0.8250833044923667758, 1.000000000000000000) ) ) 
 REPRESENTATION_ITEM ( '' )  SURFACE ( )  );
#12559 = SURFACE_SIDE_STYLE ('',( #1002 ) ) ;
#12560 = TOROIDAL_SURFACE ( 'NONE', #5939, 12.46463184759105047, 1.000000000000000000 ) ;
#12561 =( LENGTH_UNIT ( ) NAMED_UNIT ( * ) SI_UNIT ( .MILLI., .METRE. ) );
#12562 = DIRECTION ( 'NONE',  ( 0.000000000000000000, 0.000000000000000000, 1.000000000000000000 ) ) ;
#12563 = CARTESIAN_POINT ( 'NONE',  ( 0.000000000000000000, 21.75070940071369918, -13.14990448602693007 ) ) ;
#12564 = CARTESIAN_POINT ( 'NONE',  ( 76.63070922904938698, -6.859691020777852977, 76.19766410831374515 ) ) ;
#12565 = AXIS2_PLACEMENT_3D ( 'NONE', #4025, #8799, #13495 ) ;
#12566 = DIRECTION ( 'NONE',  ( -0.000000000000000000, -0.000000000000000000, -1.000000000000000000 ) ) ;
#12567 = DIRECTION ( 'NONE',  ( 1.000000000000000000, 0.000000000000000000, 0.000000000000000000 ) ) ;
#12568 = LINE ( 'NONE', #4089, #5420 ) ;
#12569 = FACE_OUTER_BOUND ( 'NONE', #3367, .T. ) ;
#12570 = AXIS2_PLACEMENT_3D ( 'NONE', #9192, #6870, #5738 ) ;
#12571 = EDGE_CURVE ( 'NONE', #5507, #5398, #1753, .T. ) ;
#12572 = CIRCLE ( 'NONE', #5954, 1.000000000000000888 ) ;
#12573 = EDGE_CURVE ( 'NONE', #8897, #9272, #10864, .T. ) ;
#12574 = ORIENTED_EDGE ( 'NONE', *, *, #15099, .T. ) ;
#12575 = LINE ( 'NONE', #9266, #12528 ) ;
#12576 = ORIENTED_EDGE ( 'NONE', *, *, #11660, .T. ) ;
#12577 = CARTESIAN_POINT ( 'NONE',  ( 75.67850768186842458, -7.475231152235347842, 72.19766410831374515 ) ) ;
#12578 = CARTESIAN_POINT ( 'NONE',  ( 51.75774672102440377, 21.75070940071325865, 139.1143251403882459 ) ) ;
#12579 = EDGE_LOOP ( 'NONE', ( #10308, #13879, #6254, #3588 ) ) ;
#12580=STYLED_ITEM('',(#15279),#14200);
#12581 = CARTESIAN_POINT ( 'NONE',  ( 120.1999296558884254, -32.15385833656369385, 53.46824312087640863 ) ) ;
#12582 = DIRECTION ( 'NONE',  ( 0.000000000000000000, 0.000000000000000000, 1.000000000000000000 ) ) ;
#12583 = AXIS2_PLACEMENT_3D ( 'NONE', #12417, #1867, #5344 ) ;
#12584 = AXIS2_PLACEMENT_3D ( 'NONE', #3342, #8043, #1033 ) ;
#12585 = CARTESIAN_POINT ( 'NONE',  ( 13.78187932340991217, -67.90279320104012584, 3.641642753176146829 ) ) ;
#12586 = CARTESIAN_POINT ( 'NONE',  ( 58.00000000000000711, -2.249290599286309256, 47.51982618741348574 ) ) ;
#12587 = CARTESIAN_POINT ( 'NONE',  ( 32.57431034208369880, -53.70580518431705741, -2.277903996697544731 ) ) ;
#12588 = CARTESIAN_POINT ( 'NONE',  ( 68.96257531573284894, -3.752529052654163255, 76.19766410831374515 ) ) ;
#12589 = DIRECTION ( 'NONE',  ( 0.8746197071345570562, -0.4848096202550665756, 0.000000000000000000 ) ) ;
#12590 = VECTOR ( 'NONE', #11041, 1000.000000000000000 ) ;
#12591 = PRODUCT_DEFINITION_SHAPE ( 'NONE', 'NONE',  #15229 ) ;
#12592 = CIRCLE ( 'NONE', #9162, 0.7892041907098322762 ) ;
#12593 = CARTESIAN_POINT ( 'NONE',  ( 96.00000000000002842, 2.750709400713692965, 139.1143251403882459 ) ) ;
#12594 = AXIS2_PLACEMENT_3D ( 'NONE', #2089, #10181, #9016 ) ;
#12595 = EDGE_LOOP ( 'NONE', ( #15132, #227, #9473, #14684 ) ) ;
#12596 = VECTOR ( 'NONE', #5918, 1000.000000000000000 ) ;
#12597 = ORIENTED_EDGE ( 'NONE', *, *, #10748, .F. ) ;
#12598 = DIRECTION ( 'NONE',  ( 1.000000000000000000, 0.000000000000000000, 0.000000000000000000 ) ) ;
#12599 = ORIENTED_EDGE ( 'NONE', *, *, #969, .T. ) ;
#12600 = CARTESIAN_POINT ( 'NONE',  ( 66.38598137497019991, -11.47113225237460910, 77.19766410831374515 ) ) ;
#12601 = CARTESIAN_POINT ( 'NONE',  ( 58.00000000000000711, -2.249290599286309256, 81.40005259842790508 ) ) ;
#12602 = VECTOR ( 'NONE', #13044, 1000.000000000000000 ) ;
#12603 = CARTESIAN_POINT ( 'NONE',  ( 55.86211336638498182, 2.337731330496643167, 62.84860122826521689 ) ) ;
#12604 = CARTESIAN_POINT ( 'NONE',  ( -12.14523415828296216, -9.827631355817223024, 48.50000000000012079 ) ) ;
#12605 = DIRECTION ( 'NONE',  ( 0.000000000000000000, 0.000000000000000000, 1.000000000000000000 ) ) ;
#12606 = ORIENTED_EDGE ( 'NONE', *, *, #3106, .T. ) ;
#12607 = AXIS2_PLACEMENT_3D ( 'NONE', #7407, #9658, #259 ) ;
#12608 = EDGE_CURVE ( 'NONE', #10969, #490, #3726, .T. ) ;
#12609 = PLANE ( 'NONE',  #2940 ) ;
#12610 = CARTESIAN_POINT ( 'NONE',  ( 9.430346510207451516, -54.59388862152623290, -3.160229925968730758 ) ) ;
#12611 = CARTESIAN_POINT ( 'NONE',  ( 52.83848824477699679, -4.298675648159541396, 60.61639468829817190 ) ) ;
#12612 = CARTESIAN_POINT ( 'NONE',  ( 114.6731053250840233, 23.25070940071369563, -33.00000000000012790 ) ) ;
#12613 = EDGE_LOOP ( 'NONE', ( #4399, #6335, #6702, #6290 ) ) ;
#12614 = CARTESIAN_POINT ( 'NONE',  ( 33.12442989620986822, -59.21224831720010684, 1.832439066040445708 ) ) ;
#12615 = EDGE_LOOP ( 'NONE', ( #7291, #10872 ) ) ;
#12616 = DIRECTION ( 'NONE',  ( -0.8586863916854874379, 0.5125013958363018318, 0.000000000000000000 ) ) ;
#12617 = PRODUCT_DEFINITION_SHAPE ( 'NONE', 'NONE',  #3261 ) ;
#12618 = ORIENTED_EDGE ( 'NONE', *, *, #9899, .F. ) ;
#12619 = AXIS2_PLACEMENT_3D ( 'NONE', #141, #5773, #15145 ) ;
#12620 = AXIS2_PLACEMENT_3D ( 'NONE', #11923, #1388, #9638 ) ;
#12621 = EDGE_CURVE ( 'NONE', #77, #1115, #12442, .T. ) ;
#12622 = EDGE_CURVE ( 'NONE', #8156, #10038, #5962, .T. ) ;
#12623 = CARTESIAN_POINT ( 'NONE',  ( -2.688903428702175252E-15, 23.25070940071368142, 139.1143251403882459 ) ) ;
#12624 = LINE ( 'NONE', #3077, #10890 ) ;
#12625 = CARTESIAN_POINT ( 'NONE',  ( 54.00000000000000711, -2.249290599286310588, 38.50000000000012790 ) ) ;
#12626 = DIRECTION ( 'NONE',  ( 0.000000000000000000, 0.000000000000000000, -1.000000000000000000 ) ) ;
#12627 = ORIENTED_EDGE ( 'NONE', *, *, #7061, .F. ) ;
#12628 = DIRECTION ( 'NONE',  ( 0.000000000000000000, 1.000000000000000000, 0.000000000000000000 ) ) ;
#12629 = DIRECTION ( 'NONE',  ( 0.8746197071345569451, -0.4848096202550666312, 0.000000000000000000 ) ) ;
#12630 = CARTESIAN_POINT ( 'NONE',  ( 69.46451111827113323, -2.308386634095125345, 75.46236687596045556 ) ) ;
#12631 = CARTESIAN_POINT ( 'NONE',  ( 62.67308791069655882, 29.52935533987996664, -33.00000000000013500 ) ) ;
#12632 = CIRCLE ( 'NONE', #14076, 5.165819364273509073 ) ;
#12633 = ORIENTED_EDGE ( 'NONE', *, *, #4576, .T. ) ;
#12634 = DIRECTION ( 'NONE',  ( -0.000000000000000000, -0.000000000000000000, -1.000000000000000000 ) ) ;
#12635 = CARTESIAN_POINT ( 'NONE',  ( -8.982583014919022446, 1.839844381040865562, 47.50000000000012079 ) ) ;
#12636 = ORIENTED_EDGE ( 'NONE', *, *, #13362, .T. ) ;
#12637 = CARTESIAN_POINT ( 'NONE',  ( 27.81410232013309525, -66.06148843087626688, -4.401172203687827356 ) ) ;
#12638 = EDGE_LOOP ( 'NONE', ( #10760, #14462 ) ) ;
#12639 =( NAMED_UNIT ( * ) PLANE_ANGLE_UNIT ( ) SI_UNIT ( $, .RADIAN. ) );
#12640 = DIRECTION ( 'NONE',  ( 1.000000000000000000, -0.000000000000000000, 0.000000000000000000 ) ) ;
#12641 = PLANE ( 'NONE',  #4736 ) ;
#12642 = VERTEX_POINT ( 'NONE', #8654 ) ;
#12643 = CARTESIAN_POINT ( 'NONE',  ( -16.99999999999998579, -2.249290599286303927, -57.50000000000012079 ) ) ;
#12644 = ADVANCED_FACE ( 'NONE', ( #14646 ), #3490, .T. ) ;
#12645 = DIRECTION ( 'NONE',  ( 0.000000000000000000, -0.000000000000000000, -1.000000000000000000 ) ) ;
#12646 = DIRECTION ( 'NONE',  ( 0.000000000000000000, 0.000000000000000000, 1.000000000000000000 ) ) ;
#12647 = DIRECTION ( 'NONE',  ( 0.8746197071345590546, -0.4848096202550629674, 0.000000000000000000 ) ) ;
#12648 = CARTESIAN_POINT ( 'NONE',  ( 53.11142512232702018, -3.558169932106523881, 48.51982618741349285 ) ) ;
#12649 = ORIENTED_EDGE ( 'NONE', *, *, #14162, .F. ) ;
#12650 = CARTESIAN_POINT ( 'NONE',  ( -25.46282903980766932, -6.565599745187317815, 58.00000000000012079 ) ) ;
#12651 = VERTEX_POINT ( 'NONE', #7656 ) ;
#12652 = CARTESIAN_POINT ( 'NONE',  ( 29.70251902843243741, -52.24929059928630437, -4.175384597093465544 ) ) ;
#12653 = CARTESIAN_POINT ( 'NONE',  ( 40.33162949095117966, 0.000000000000000000, 139.1143251403882459 ) ) ;
#12654 = ORIENTED_EDGE ( 'NONE', *, *, #12622, .T. ) ;
#12655 = DIRECTION ( 'NONE',  ( 1.000000000000000000, 0.000000000000000000, 0.000000000000000000 ) ) ;
#12656 = CARTESIAN_POINT ( 'NONE',  ( 52.94134894379979528, -2.395505968190773327, 62.84860122826521689 ) ) ;
#12657 = B_SPLINE_CURVE_WITH_KNOTS ( 'NONE', 3,
 ( #6715, #783, #14793, #13793, #11399, #14869, #5566, #5645, #4561, #10337, #1015, #5735, #15032, #10261, #4484, #7798, #12491, #4247 ),
 .UNSPECIFIED., .F., .F.,
 ( 4, 2, 2, 2, 2, 2, 2, 2, 4 ),
 ( 0.000000000000000000, 0.0007591815323294819756, 0.001518363064658963951, 0.002277544596988445493, 0.003036726129317927902, 0.003795907661647409878, 0.004555089193976890986, 0.005314270726306382503, 0.006073452258635873152 ),
 .UNSPECIFIED. ) ;
#12658 = DIRECTION ( 'NONE',  ( 0.000000000000000000, 0.000000000000000000, 1.000000000000000000 ) ) ;
#12659 = ADVANCED_FACE ( 'NONE', ( #10971 ), #13351, .T. ) ;
#12660 = ADVANCED_FACE ( 'NONE', ( #8582 ), #13415, .T. ) ;
#12661 = DIRECTION ( 'NONE',  ( 0.5394184268574535590, -0.8420378618367644341, 0.000000000000000000 ) ) ;
#12662 =( REPRESENTATION_RELATIONSHIP ('NONE','NONE', #15125, #11466 ) REPRESENTATION_RELATIONSHIP_WITH_TRANSFORMATION ( #13386 )SHAPE_REPRESENTATION_RELATIONSHIP( ) );
#12663 = CARTESIAN_POINT ( 'NONE',  ( 32.43636434651678258, -59.39117099671923228, 2.764779704643939073 ) ) ;
#12664 = DIRECTION ( 'NONE',  ( -0.8746197071345572782, 0.4848096202550659650, -0.000000000000000000 ) ) ;
#12665 = DIRECTION ( 'NONE',  ( -0.000000000000000000, -0.000000000000000000, 1.000000000000000000 ) ) ;
#12666 = DIRECTION ( 'NONE',  ( -0.000000000000000000, 1.000000000000000000, -0.000000000000000000 ) ) ;
#12667 = ORIENTED_EDGE ( 'NONE', *, *, #2058, .T. ) ;
#12668 = CARTESIAN_POINT ( 'NONE',  ( 6.635030218769952803, -47.02811197266219523, -2.732446379177816187 ) ) ;
#12669 = VERTEX_POINT ( 'NONE', #6565 ) ;
#12670 = DIRECTION ( 'NONE',  ( 0.000000000000000000, -0.000000000000000000, -1.000000000000000000 ) ) ;
#12671 = ORIENTED_EDGE ( 'NONE', *, *, #15218, .F. ) ;
#12672 = SURFACE_STYLE_USAGE ( .BOTH. , #11589 ) ;
#12673 = DIRECTION ( 'NONE',  ( -0.8656763553493057595, -0.5006040828730249359, 0.000000000000000000 ) ) ;
#12674 = B_SPLINE_CURVE_WITH_KNOTS ( 'NONE', 3,
 ( #1484, #13114, #8421, #13182, #2569, #7256, #2637, #12019, #10879, #13393 ),
 .UNSPECIFIED., .F., .F.,
 ( 4, 2, 2, 2, 4 ),
 ( 0.000000000000000000, 0.0003835113287520874100, 0.0007670226575041748200, 0.001150533986256262230, 0.001534045315008349640 ),
 .UNSPECIFIED. ) ;
#12675 = EDGE_CURVE ( 'NONE', #8736, #4237, #2812, .T. ) ;
#12676 = VECTOR ( 'NONE', #255, 1000.000000000000000 ) ;
#12677 = DIRECTION ( 'NONE',  ( -0.000000000000000000, -0.000000000000000000, 1.000000000000000000 ) ) ;
#12678 = CARTESIAN_POINT ( 'NONE',  ( 109.8334623555409735, 0.000000000000000000, -13.14990448602693007 ) ) ;
#12679 = ORIENTED_EDGE ( 'NONE', *, *, #881, .T. ) ;
#12680 = CARTESIAN_POINT ( 'NONE',  ( 58.00000000000000711, -2.249290599286309256, 87.40005259842790508 ) ) ;
#12681 = VERTEX_POINT ( 'NONE', #4102 ) ;
#12682 = CARTESIAN_POINT ( 'NONE',  ( 80.00000000000001421, -87.24929059928631148, -35.00000000000000000 ) ) ;
#12683 = CARTESIAN_POINT ( 'NONE',  ( 8.201103799357261082, -57.48563641131178770, -1.816685854991394455 ) ) ;
#12684 = DIRECTION ( 'NONE',  ( -0.8208219420614785156, 0.4549890321264268844, 0.3453061251629924167 ) ) ;
#12685 = CARTESIAN_POINT ( 'NONE',  ( -10.04144563215826835, -7.967033079555101871, 47.93156476714629122 ) ) ;
#12686 = EDGE_LOOP ( 'NONE', ( #11216, #1149, #10416, #12742 ) ) ;
#12687 = VECTOR ( 'NONE', #514, 1000.000000000000000 ) ;
#12688 = FACE_OUTER_BOUND ( 'NONE', #5153, .T. ) ;
#12689 = VERTEX_POINT ( 'NONE', #3042 ) ;
#12690 = DIRECTION ( 'NONE',  ( -1.000000000000000000, -1.156482317317870492E-16, 0.000000000000000000 ) ) ;
#12691 = ORIENTED_EDGE ( 'NONE', *, *, #10794, .T. ) ;
#12692 = DIRECTION ( 'NONE',  ( -0.000000000000000000, 1.000000000000000000, 1.445602896647339163E-16 ) ) ;
#12693 = CARTESIAN_POINT ( 'NONE',  ( -25.15752072101216896, 2.619472661158628313, -48.00000000000012079 ) ) ;
#12694 = VERTEX_POINT ( 'NONE', #10042 ) ;
#12695 = AXIS2_PLACEMENT_3D ( 'NONE', #756, #8995, #11226 ) ;
#12696 = LINE ( 'NONE', #12545, #12940 ) ;
#12697 = VECTOR ( 'NONE', #3205, 1000.000000000000000 ) ;
#12698 = FILL_AREA_STYLE_COLOUR ( '', #5451 ) ;
#12699 = EDGE_CURVE ( 'NONE', #8918, #7187, #14545, .T. ) ;
#12700 = ORIENTED_EDGE ( 'NONE', *, *, #7723, .F. ) ;
#12701 = FACE_OUTER_BOUND ( 'NONE', #1410, .T. ) ;
#12702 = CARTESIAN_POINT ( 'NONE',  ( 56.97758043373130477, 2.707118148285912795, 60.61639468829817190 ) ) ;
#12703 = PLANE ( 'NONE',  #14488 ) ;
#12704 = AXIS2_PLACEMENT_3D ( 'NONE', #7517, #11268, #14520 ) ;
#12705 = ADVANCED_FACE ( 'NONE', ( #14725 ), #4026, .T. ) ;
#12706 = CARTESIAN_POINT ( 'NONE',  ( 67.15257324181105503, -7.322644791425997113, 60.61639468829817190 ) ) ;
#12707 = CARTESIAN_POINT ( 'NONE',  ( 29.14554934997181590, -50.05638191677163462, 4.212312498554270590 ) ) ;
#12708 = EDGE_CURVE ( 'NONE', #864, #11054, #5716, .T. ) ;
#12709 = ORIENTED_EDGE ( 'NONE', *, *, #364, .T. ) ;
#12710 = EDGE_CURVE ( 'NONE', #7295, #10265, #12846, .T. ) ;
#12711 = CARTESIAN_POINT ( 'NONE',  ( 70.13908301581606963, -3.720822497039482979, 72.39370326752943186 ) ) ;
#12712 = VECTOR ( 'NONE', #191, 1000.000000000000000 ) ;
#12713 = CARTESIAN_POINT ( 'NONE',  ( -3.190546569013415379, 0.8906624217387615339, 48.00000000000012079 ) ) ;
#12714 = EDGE_LOOP ( 'NONE', ( #434, #2765, #8409, #5893 ) ) ;
#12715 = CARTESIAN_POINT ( 'NONE',  ( 0.000000000000000000, 21.75070940071312364, 139.1143251403882459 ) ) ;
#12716 = DIRECTION ( 'NONE',  ( -0.000000000000000000, -0.000000000000000000, -1.000000000000000000 ) ) ;
#12717 = EDGE_CURVE ( 'NONE', #307, #9321, #12348, .T. ) ;
#12718 =( NAMED_UNIT ( * ) SI_UNIT ( $, .STERADIAN. ) SOLID_ANGLE_UNIT ( ) );
#12719 = CARTESIAN_POINT ( 'NONE',  ( -9.456985518117400957, -7.172040337370347629, -47.50000001881890910 ) ) ;
#12720 = DIRECTION ( 'NONE',  ( -1.000000000000000000, 0.000000000000000000, 0.000000000000000000 ) ) ;
#12721 = ORIENTED_EDGE ( 'NONE', *, *, #5039, .F. ) ;
#12722 = VECTOR ( 'NONE', #13224, 1000.000000000000000 ) ;
#12723 = FACE_OUTER_BOUND ( 'NONE', #8150, .T. ) ;
#12724 = PLANE ( 'NONE',  #9492 ) ;
#12725 = AXIS2_PLACEMENT_3D ( 'NONE', #11575, #12904, #3427 ) ;
#12726 = AXIS2_PLACEMENT_3D ( 'NONE', #7479, #11157, #14692 ) ;
#12727 = DIRECTION ( 'NONE',  ( 0.000000000000000000, 0.000000000000000000, -1.000000000000000000 ) ) ;
#12728 = CARTESIAN_POINT ( 'NONE',  ( 11.11753584644737280, -62.41236107492795782, 2.580051240451665784 ) ) ;
#12729 = DIRECTION ( 'NONE',  ( 1.000000000000000000, -6.938893903907228378E-17, 0.000000000000000000 ) ) ;
#12730 = CYLINDRICAL_SURFACE ( 'NONE', #13540, 0.7892041907098262810 ) ;
#12731 = EDGE_CURVE ( 'NONE', #14173, #4038, #11039, .T. ) ;
#12732 = ORIENTED_EDGE ( 'NONE', *, *, #10509, .T. ) ;
#12733 = VECTOR ( 'NONE', #11417, 1000.000000000000000 ) ;
#12734 = ORIENTED_EDGE ( 'NONE', *, *, #13570, .F. ) ;
#12735 = CARTESIAN_POINT ( 'NONE',  ( 27.84032651173070860, -68.65142943889377136, -4.053691724355999781 ) ) ;
#12736 = EDGE_CURVE ( 'NONE', #10906, #977, #13283, .T. ) ;
#12737 = ORIENTED_EDGE ( 'NONE', *, *, #10358, .F. ) ;
#12738 = FACE_OUTER_BOUND ( 'NONE', #12518, .T. ) ;
#12739 = CARTESIAN_POINT ( 'NONE',  ( 11.81201825756313539, -52.27654955159783157, 3.048121150676241786 ) ) ;
#12740 = AXIS2_PLACEMENT_3D ( 'NONE', #9419, #14110, #3562 ) ;
#12741 = CIRCLE ( 'NONE', #6804, 0.4999999999999999445 ) ;
#12742 = ORIENTED_EDGE ( 'NONE', *, *, #12109, .T. ) ;
#12743 = CARTESIAN_POINT ( 'NONE',  ( -2.688903428702175252E-15, 23.25070940071368142, -33.00000000000012790 ) ) ;
#12744 = PLANE ( 'NONE',  #13447 ) ;
#12745 = CARTESIAN_POINT ( 'NONE',  ( 13.86157779355430186, -69.45278782524461292, 3.616934341765148719 ) ) ;
#12746 = VECTOR ( 'NONE', #12634, 1000.000000000000000 ) ;
#12747 = DIRECTION ( 'NONE',  ( 0.8746197071345590546, -0.4848096202550629674, 0.000000000000000000 ) ) ;
#12748 = CARTESIAN_POINT ( 'NONE',  ( 31.99980918299992538, -53.15380395407657232, -2.455672049130702028 ) ) ;
#12749 = LINE ( 'NONE', #3192, #5427 ) ;
#12750 = EDGE_CURVE ( 'NONE', #4753, #15091, #7191, .T. ) ;
#12751 = VECTOR ( 'NONE', #5753, 1000.000000000000000 ) ;
#12752 = CARTESIAN_POINT ( 'NONE',  ( 9.236734562794072900, -59.22985212983980574, 2.757908476812879872 ) ) ;
#12753 = CARTESIAN_POINT ( 'NONE',  ( -25.40901433244242114, -6.686340856221296036, -48.00000000000012079 ) ) ;
#12754 = ORIENTED_EDGE ( 'NONE', *, *, #7486, .F. ) ;
#12755 = B_SPLINE_CURVE_WITH_KNOTS ( 'NONE', 3,
 ( #5465, #10159, #6898, #15137, #12458, #6386, #13985, #1914 ),
 .UNSPECIFIED., .F., .F.,
 ( 4, 2, 2, 4 ),
 ( 0.000000000000000000, 0.0002685324218445792163, 0.0005370648436891596253, 0.001074129687378317299 ),
 .UNSPECIFIED. ) ;
#12756 = CARTESIAN_POINT ( 'NONE',  ( -12.83418063572647760, -2.249290599286303927, 50.50000000000012079 ) ) ;
#12757 = EDGE_CURVE ( 'NONE', #1708, #4049, #1805, .T. ) ;
#12758 = EDGE_CURVE ( 'NONE', #6921, #4603, #12269, .T. ) ;
#12759 = ORIENTED_EDGE ( 'NONE', *, *, #2311, .T. ) ;
#12760 = CARTESIAN_POINT ( 'NONE',  ( -28.70947653109703168, -9.020656969121420232, 48.50000000000012079 ) ) ;
#12761 = ORIENTED_EDGE ( 'NONE', *, *, #10646, .F. ) ;
#12762 = CARTESIAN_POINT ( 'NONE',  ( -16.99999999999998579, 7.750709400713696517, 33.00000000000012790 ) ) ;
#12763 = LINE ( 'NONE', #14065, #13678 ) ;
#12764 = CARTESIAN_POINT ( 'NONE',  ( 16.17808712815840266, -52.24929059925523234, -5.670202843295511386 ) ) ;
#12765 = ORIENTED_EDGE ( 'NONE', *, *, #2820, .T. ) ;
#12766 = CARTESIAN_POINT ( 'NONE',  ( -80.00000000000001421, -74.24929059928631148, -32.00000000000000000 ) ) ;
#12767 = CARTESIAN_POINT ( 'NONE',  ( 10.00121363803638808, -52.94991738523399505, -2.538129127158726739 ) ) ;
#12768 = DIRECTION ( 'NONE',  ( 0.000000000000000000, -0.000000000000000000, 1.000000000000000000 ) ) ;
#12769 = CARTESIAN_POINT ( 'NONE',  ( -8.842479278987875446, -7.118053859731355182, 48.00000000000012079 ) ) ;
#12770 = AXIS2_PLACEMENT_3D ( 'NONE', #14112, #11715, #8192 ) ;
#12771 = VERTEX_POINT ( 'NONE', #6280 ) ;
#12772 = ORIENTED_EDGE ( 'NONE', *, *, #8937, .T. ) ;
#12773 = EDGE_CURVE ( 'NONE', #7237, #8156, #14315, .T. ) ;
#12774 = ADVANCED_FACE ( 'NONE', ( #6419 ), #11116, .F. ) ;
#12775 = CARTESIAN_POINT ( 'NONE',  ( -25.46282903980766932, -6.565599745187317815, -57.50000000000012079 ) ) ;
#12776 = VERTEX_POINT ( 'NONE', #5744 ) ;
#12777 = DIRECTION ( 'NONE',  ( -0.000000000000000000, 0.000000000000000000, -1.000000000000000000 ) ) ;
#12778 = VERTEX_POINT ( 'NONE', #7964 ) ;
#12779 = VERTEX_POINT ( 'NONE', #11486 ) ;
#12780 = CARTESIAN_POINT ( 'NONE',  ( 53.19261734817368392, 0.4154851184807644149, 82.40005259842790508 ) ) ;
#12781 = CARTESIAN_POINT ( 'NONE',  ( 23.10474973039555735, -53.24929059928630437, 5.564967562786288902 ) ) ;
#12782 = EDGE_LOOP ( 'NONE', ( #12432, #5698, #10723, #13620 ) ) ;
#12783 = CIRCLE ( 'NONE', #14252, 4.000000000000000000 ) ;
#12784 = VECTOR ( 'NONE', #278, 1000.000000000000000 ) ;
#12785 = CARTESIAN_POINT ( 'NONE',  ( 8.990236908599356980, -55.34783937825962141, -2.956317232382419835 ) ) ;
#12786 = DIRECTION ( 'NONE',  ( 0.000000000000000000, 0.000000000000000000, -1.000000000000000000 ) ) ;
#12787 = ORIENTED_EDGE ( 'NONE', *, *, #7582, .T. ) ;
#12788 = CARTESIAN_POINT ( 'NONE',  ( -1.243300532054838308E-15, 10.75070940071368142, 33.00000000000012790 ) ) ;
#12789 = DIRECTION ( 'NONE',  ( 0.3583679495359998191, -0.9335804265007718872, 0.000000000000000000 ) ) ;
#12790 = CARTESIAN_POINT ( 'NONE',  ( 25.54537353428280611, -52.24929059928630437, 5.670202843357490252 ) ) ;
#12791 = CARTESIAN_POINT ( 'NONE',  ( 24.27245784421982222, -72.28366650276025496, 6.113054590620157214 ) ) ;
#12792 = VERTEX_POINT ( 'NONE', #2187 ) ;
#12793 = CARTESIAN_POINT ( 'NONE',  ( 20.86173033120691045, -53.24929059928630437, 6.000000000000000000 ) ) ;
#12794 = VECTOR ( 'NONE', #11913, 1000.000000000000000 ) ;
#12795 = EDGE_CURVE ( 'NONE', #3738, #14936, #10272, .T. ) ;
#12796 = ORIENTED_EDGE ( 'NONE', *, *, #11895, .T. ) ;
#12797 = DIRECTION ( 'NONE',  ( -1.000000000000000000, 5.551115123125787632E-16, 0.000000000000000000 ) ) ;
#12798 = CARTESIAN_POINT ( 'NONE',  ( -8.787473001628837821, 2.499856724289235554, 48.50000000000012079 ) ) ;
#12799 = DIRECTION ( 'NONE',  ( 0.000000000000000000, 0.000000000000000000, 1.000000000000000000 ) ) ;
#12800 = CARTESIAN_POINT ( 'NONE',  ( -10.04144563215826835, -7.967033079554944663, -47.93156476714629122 ) ) ;
#12801 = CARTESIAN_POINT ( 'NONE',  ( -11.83418063572647760, -2.249290599286303927, 57.50000000000012079 ) ) ;
#12802 = ORIENTED_EDGE ( 'NONE', *, *, #2587, .F. ) ;
#12803 = DIRECTION ( 'NONE',  ( 1.000000000000000000, 0.000000000000000000, 0.000000000000000000 ) ) ;
#12804 = DIRECTION ( 'NONE',  ( -0.000000000000000000, 1.000000000000000000, 1.445602896647339163E-16 ) ) ;
#12805 = CIRCLE ( 'NONE', #4177, 4.194885682587998765 ) ;
#12807 = EDGE_CURVE ( 'NONE', #7606, #14840, #12592, .T. ) ;
#12806 = DIRECTION ( 'NONE',  ( -0.5394184268574404584, 0.8420378618367728718, 0.000000000000000000 ) ) ;
#12808 = CARTESIAN_POINT ( 'NONE',  ( 80.00000000000001421, -85.24929059928631148, 6.000000000000001776 ) ) ;
#12809 = DIRECTION ( 'NONE',  ( 0.000000000000000000, 0.000000000000000000, 1.000000000000000000 ) ) ;
#12810 = EDGE_CURVE ( 'NONE', #11258, #1460, #10429, .T. ) ;
#12811 = EDGE_LOOP ( 'NONE', ( #8114, #8274, #7224, #3609 ) ) ;
#12812 = AXIS2_PLACEMENT_3D ( 'NONE', #13606, #6519, #5375 ) ;
#12813 = DIRECTION ( 'NONE',  ( 0.000000000000000000, 0.000000000000000000, -1.000000000000000000 ) ) ;
#12814 = ORIENTED_EDGE ( 'NONE', *, *, #1226, .T. ) ;
#12815 = DIRECTION ( 'NONE',  ( 0.9839406800755992055, -0.1784957649143736891, 0.000000000000000000 ) ) ;
#12816 = CARTESIAN_POINT ( 'NONE',  ( 8.987770063152476396, -53.89143413596318055, 2.226202503535223531 ) ) ;
#12817 = ORIENTED_EDGE ( 'NONE', *, *, #8948, .T. ) ;
#12818 = DIRECTION ( 'NONE',  ( -0.000000000000000000, 0.000000000000000000, -1.000000000000000000 ) ) ;
#12819 = FACE_OUTER_BOUND ( 'NONE', #14875, .T. ) ;
#12820 = ADVANCED_FACE ( 'NONE', ( #11564 ), #2102, .T. ) ;
#12821 = EDGE_CURVE ( 'NONE', #8129, #6079, #11789, .T. ) ;
#12822 = AXIS2_PLACEMENT_3D ( 'NONE', #3222, #7925, #12616 ) ;
#12823 = DIRECTION ( 'NONE',  ( 0.000000000000000000, 0.000000000000000000, 1.000000000000000000 ) ) ;
#12824 = VECTOR ( 'NONE', #8479, 1000.000000000000000 ) ;
#12825 = PLANE ( 'NONE',  #1174 ) ;
#12826 = FACE_OUTER_BOUND ( 'NONE', #14580, .T. ) ;
#12827 = CARTESIAN_POINT ( 'NONE',  ( -16.99999999999998579, -2.249290599286303927, 47.50000000000012079 ) ) ;
#12828 = CYLINDRICAL_SURFACE ( 'NONE', #2306, 4.505436745857433145 ) ;
#12829 = CARTESIAN_POINT ( 'NONE',  ( -21.85476584171713199, 5.329050157244537900, -48.50000000000012079 ) ) ;
#12830 = ORIENTED_EDGE ( 'NONE', *, *, #1361, .T. ) ;
#12831 = DIRECTION ( 'NONE',  ( 0.000000000000000000, 0.000000000000000000, 1.000000000000000000 ) ) ;
#12832 = VECTOR ( 'NONE', #15119, 1000.000000000000000 ) ;
#12833 = VECTOR ( 'NONE', #738, 1000.000000000000000 ) ;
#12834 = ORIENTED_EDGE ( 'NONE', *, *, #5411, .T. ) ;
#12835 = DIRECTION ( 'NONE',  ( 0.000000000000000000, -0.000000000000000000, -1.000000000000000000 ) ) ;
#12836 = AXIS2_PLACEMENT_3D ( 'NONE', #2230, #7566, #8999 ) ;
#12837 = ORIENTED_EDGE ( 'NONE', *, *, #15073, .F. ) ;
#12838 = CARTESIAN_POINT ( 'NONE',  ( 70.46453521882889959, -2.298370886119723622, 82.40005259842790508 ) ) ;
#12839 = ORIENTED_EDGE ( 'NONE', *, *, #8938, .F. ) ;
#12840 = CARTESIAN_POINT ( 'NONE',  ( 64.48276670783141640, -11.70694761207440671, 76.45535061892491058 ) ) ;
#12841 = FACE_OUTER_BOUND ( 'NONE', #1888, .T. ) ;
#12842 = DIRECTION ( 'NONE',  ( 0.8208219420614785156, -0.4549890321264269399, -0.3453061251629920836 ) ) ;
#12843 = AXIS2_PLACEMENT_3D ( 'NONE', #3408, #3327, #11550 ) ;
#12844 = PRESENTATION_LAYER_ASSIGNMENT (  '', '', ( #7176 ) ) ;
#12845 = ORIENTED_EDGE ( 'NONE', *, *, #5525, .T. ) ;
#12846 = CIRCLE ( 'NONE', #3981, 7.924024642120691908 ) ;
#12847 = ADVANCED_FACE ( 'NONE', ( #8957 ), #14801, .F. ) ;
#12848 = CIRCLE ( 'NONE', #6216, 0.7892041907098290565 ) ;
#12849 = DIRECTION ( 'NONE',  ( 1.000000000000000000, 0.000000000000000000, 0.000000000000000000 ) ) ;
#12850 = CARTESIAN_POINT ( 'NONE',  ( 9.159236525127615991, -55.01088356445123395, -3.038469202939837466 ) ) ;
#12851 = LINE ( 'NONE', #13910, #12358 ) ;
#12852 = EDGE_CURVE ( 'NONE', #6792, #7944, #3104, .T. ) ;
#12853 = LINE ( 'NONE', #6991, #1069 ) ;
#12854 = EDGE_LOOP ( 'NONE', ( #2838, #10623, #5578, #9203, #4922 ) ) ;
#12855 = CARTESIAN_POINT ( 'NONE',  ( 33.12582565096496978, -59.20619211347772648, 2.502190571104487393 ) ) ;
#12856 = VERTEX_POINT ( 'NONE', #13884 ) ;
#12857 = CARTESIAN_POINT ( 'NONE',  ( 13.47393939923805561, -64.89111109908232322, 4.244693487287860556 ) ) ;
#12858 = ORIENTED_EDGE ( 'NONE', *, *, #4052, .F. ) ;
#12859 = CIRCLE ( 'NONE', #14798, 3.694885682587998765 ) ;
#12860 = VERTEX_POINT ( 'NONE', #6644 ) ;
#12861 = AXIS2_PLACEMENT_3D ( 'NONE', #9469, #8392, #2541 ) ;
#12862 = CARTESIAN_POINT ( 'NONE',  ( -12.99999999999998757, -2.249290599286303483, 33.00000000000012790 ) ) ;
#12863 = FACE_OUTER_BOUND ( 'NONE', #11040, .T. ) ;
#12864 = ORIENTED_EDGE ( 'NONE', *, *, #14768, .F. ) ;
#12865 = AXIS2_PLACEMENT_3D ( 'NONE', #3234, #11456, #7937 ) ;
#12866 = CARTESIAN_POINT ( 'NONE',  ( 62.30678795759143185, -4.906903613034745426, 60.61639468829817190 ) ) ;
#12867 = CARTESIAN_POINT ( 'NONE',  ( 70.17731411157174648, -3.883646954095939741, 72.30896232854578898 ) ) ;
#12868 = EDGE_CURVE ( 'NONE', #7803, #777, #2268, .T. ) ;
#12869 = ORIENTED_EDGE ( 'NONE', *, *, #8747, .T. ) ;
#12870 = EDGE_CURVE ( 'NONE', #11623, #8078, #4411, .T. ) ;
#12871 = CARTESIAN_POINT ( 'NONE',  ( -7.999999999999986677, -2.249290599286305259, -38.50000000000012790 ) ) ;
#12872 = DIRECTION ( 'NONE',  ( 0.8746197071345569451, -0.4848096202550666312, 0.000000000000000000 ) ) ;
#12873 = CARTESIAN_POINT ( 'NONE',  ( 29.35555050496136076, -52.24929059928630437, 3.199931146564416462 ) ) ;
#12874 = CARTESIAN_POINT ( 'NONE',  ( -16.99999999999998579, -2.249290599286303927, 36.00000000000012079 ) ) ;
#12875 = VERTEX_POINT ( 'NONE', #7884 ) ;
#12876 = CIRCLE ( 'NONE', #13347, 1.000000000000007550 ) ;
#12877 = CARTESIAN_POINT ( 'NONE',  ( 18.61871093201826000, -52.24929059928630437, 5.564967562786272914 ) ) ;
#12878 = VECTOR ( 'NONE', #5152, 1000.000000000000000 ) ;
#12879 = VERTEX_POINT ( 'NONE', #3183 ) ;
#12880 = FACE_OUTER_BOUND ( 'NONE', #6718, .T. ) ;
#12881 = FILL_AREA_STYLE ('',( #13024 ) ) ;
#12882 = EDGE_LOOP ( 'NONE', ( #8350, #10132, #13854, #1161 ) ) ;
#12883 = DIRECTION ( 'NONE',  ( 0.000000000000000000, 0.000000000000000000, 1.000000000000000000 ) ) ;
#12884 = DIRECTION ( 'NONE',  ( -0.000000000000000000, 1.000000000000000000, 1.445602896647339163E-16 ) ) ;
#12885 = CARTESIAN_POINT ( 'NONE',  ( 31.72322230991231962, -61.42570632716525125, 2.132522520905362651 ) ) ;
#12886 = ORIENTED_EDGE ( 'NONE', *, *, #4034, .F. ) ;
#12887 = EDGE_CURVE ( 'NONE', #1549, #5437, #2029, .T. ) ;
#12888 = CARTESIAN_POINT ( 'NONE',  ( 43.00000000000000711, 10.25070940071368497, 139.1143251403882459 ) ) ;
#12889 = VECTOR ( 'NONE', #13585, 1000.000000000000000 ) ;
#12890 = CARTESIAN_POINT ( 'NONE',  ( 32.36512860216036103, -60.82697974174514144, -1.965378744864697103 ) ) ;
#12891 = CARTESIAN_POINT ( 'NONE',  ( 9.369695877296390307, -60.81027516727737492, 1.970305681586464130 ) ) ;
#12892 = CARTESIAN_POINT ( 'NONE',  ( 114.6731053250840233, 0.000000000000000000, 33.00000000000012790 ) ) ;
#12893 = DIRECTION ( 'NONE',  ( -0.000000000000000000, 1.000000000000000000, -0.000000000000000000 ) ) ;
#12894 = FACE_OUTER_BOUND ( 'NONE', #8986, .T. ) ;
#12895 = ORIENTED_EDGE ( 'NONE', *, *, #6036, .F. ) ;
#12896 = CARTESIAN_POINT ( 'NONE',  ( -65.00000000000001421, -85.24929059928631148, 19.99999999999999645 ) ) ;
#12897 = ORIENTED_EDGE ( 'NONE', *, *, #570, .T. ) ;
#12898 = CARTESIAN_POINT ( 'NONE',  ( 27.55953187330915810, 23.25070940071368852, 33.00000000000012790 ) ) ;
#12899 = CARTESIAN_POINT ( 'NONE',  ( -80.00000000000001421, -76.24929059928631148, -4.000000000000000000 ) ) ;
#12900 = ORIENTED_EDGE ( 'NONE', *, *, #6966, .T. ) ;
#12901 = CARTESIAN_POINT ( 'NONE',  ( 30.65234355186507997, 23.25070940071368852, -33.00000000000012790 ) ) ;
#12902 = CARTESIAN_POINT ( 'NONE',  ( 47.27423575335444639, 25.52935533987996664, 84.20452624982236500 ) ) ;
#12903 = FACE_OUTER_BOUND ( 'NONE', #5232, .T. ) ;
#12904 = DIRECTION ( 'NONE',  ( -9.912705577010325549E-17, 1.734723475976817547E-15, -1.000000000000000000 ) ) ;
#12905 = CARTESIAN_POINT ( 'NONE',  ( -26.99999999999998224, -72.24929059928631148, -115.4621125123531442 ) ) ;
#12906 = CARTESIAN_POINT ( 'NONE',  ( -24.60804510916187837, -7.057608296800744085, 47.99579695943414492 ) ) ;
#12907 = CARTESIAN_POINT ( 'NONE',  ( 13.86173033120690334, -69.39711819508848123, 3.801276035476828685 ) ) ;
#12908 = CARTESIAN_POINT ( 'NONE',  ( 31.69392142191828299, -52.92218391219104490, 3.457912412235188082 ) ) ;
#12909 = EDGE_CURVE ( 'NONE', #4896, #10195, #853, .T. ) ;
#12910 = ORIENTED_EDGE ( 'NONE', *, *, #4862, .F. ) ;
#12911 = EDGE_CURVE ( 'NONE', #6655, #9231, #14810, .T. ) ;
#12912 = EDGE_CURVE ( 'NONE', #8264, #5832, #9587, .T. ) ;
#12913 = CARTESIAN_POINT ( 'NONE',  ( 71.15942379059755751, -15.26044865788734484, 72.19766410831374515 ) ) ;
#12914 = ORIENTED_EDGE ( 'NONE', *, *, #9328, .F. ) ;
#12915 = CARTESIAN_POINT ( 'NONE',  ( 20.86173033120691045, -57.24929059928630437, -3.000000000000000888 ) ) ;
#12916 = ORIENTED_EDGE ( 'NONE', *, *, #663, .T. ) ;
#12917 = ORIENTED_EDGE ( 'NONE', *, *, #1346, .T. ) ;
#12918 = CARTESIAN_POINT ( 'NONE',  ( 65.08836494111386628, -11.27206642318173735, 76.12732364699549237 ) ) ;
#12919 = DIRECTION ( 'NONE',  ( 0.000000000000000000, 0.000000000000000000, 1.000000000000000000 ) ) ;
#12920 = EDGE_CURVE ( 'NONE', #13229, #5503, #8427, .T. ) ;
#12921 = CARTESIAN_POINT ( 'NONE',  ( 12.03298173962126860, -53.28399145779480506, -4.141535524925034295 ) ) ;
#12922 = ORIENTED_EDGE ( 'NONE', *, *, #13831, .T. ) ;
#12923 = CARTESIAN_POINT ( 'NONE',  ( 58.00000000000000711, -2.249290599286311032, 33.00000000000012790 ) ) ;
#12924 = DIRECTION ( 'NONE',  ( 0.8420378618367735379, 0.5394184268574396812, 9.357418084440779321E-16 ) ) ;
#12925 = CARTESIAN_POINT ( 'NONE',  ( -3.190546569013415379, 0.8906624217387615339, 48.00000000000012079 ) ) ;
#12926 = ORIENTED_EDGE ( 'NONE', *, *, #9519, .F. ) ;
#12927 = EDGE_LOOP ( 'NONE', ( #6739, #8513, #883, #2301, #3633, #5746, #14196, #11000, #811, #14759, #12654, #14329 ) ) ;
#12928 = CARTESIAN_POINT ( 'NONE',  ( 20.86173033120691045, -52.24929059928630437, 0.000000000000000000 ) ) ;
#12929 = ORIENTED_EDGE ( 'NONE', *, *, #622, .F. ) ;
#12930 = FACE_OUTER_BOUND ( 'NONE', #13498, .T. ) ;
#12931 = ORIENTED_EDGE ( 'NONE', *, *, #5395, .F. ) ;
#12932 = ADVANCED_FACE ( 'NONE', ( #8354 ), #4731, .T. ) ;
#12933 = ORIENTED_EDGE ( 'NONE', *, *, #13360, .T. ) ;
#12934 = CARTESIAN_POINT ( 'NONE',  ( 52.35373241494735197, -0.8423457118892130335, 62.84860122826521689 ) ) ;
#12935 = CARTESIAN_POINT ( 'NONE',  ( 45.17127246049422240, 0.000000000000000000, 139.1143251403882459 ) ) ;
#12936 = ORIENTED_EDGE ( 'NONE', *, *, #8831, .T. ) ;
#12937 = CARTESIAN_POINT ( 'NONE',  ( 0.000000000000000000, 0.000000000000000000, 38.00000000000012079 ) ) ;
#12938 = DIRECTION ( 'NONE',  ( -1.000000000000000000, 0.000000000000000000, 0.000000000000000000 ) ) ;
#12939 = VERTEX_POINT ( 'NONE', #9504 ) ;
#12940 = VECTOR ( 'NONE', #2148, 1000.000000000000000 ) ;
#12941 = DIRECTION ( 'NONE',  ( 0.000000000000000000, 1.927470528863120035E-16, -1.000000000000000000 ) ) ;
#12942 = CARTESIAN_POINT ( 'NONE',  ( 20.86173033120691045, -74.24929059928636832, 0.000000000000000000 ) ) ;
#12943 = CARTESIAN_POINT ( 'NONE',  ( 73.69809405469877106, 29.52935533987996664, -21.00807340887166674 ) ) ;
#12944 = FACE_OUTER_BOUND ( 'NONE', #10541, .T. ) ;
#12945 = ORIENTED_EDGE ( 'NONE', *, *, #2521, .F. ) ;
#12946 = CARTESIAN_POINT ( 'NONE',  ( 69.36166834748301824, -3.800326805936743213, 71.24799951533148601 ) ) ;
#12947 = EDGE_CURVE ( 'NONE', #1277, #10836, #14352, .T. ) ;
#12948 = ORIENTED_EDGE ( 'NONE', *, *, #7672, .T. ) ;
#12949 = EDGE_CURVE ( 'NONE', #59, #4156, #9893, .T. ) ;
#12950 = CARTESIAN_POINT ( 'NONE',  ( 80.00000000000001421, -74.24929059928631148, 8.000000000000001776 ) ) ;
#12951 = DIRECTION ( 'NONE',  ( -0.000000000000000000, 0.000000000000000000, -1.000000000000000000 ) ) ;
#12952 = DIRECTION ( 'NONE',  ( 1.000000000000000000, 0.000000000000000000, 0.000000000000000000 ) ) ;
#12953 = CARTESIAN_POINT ( 'NONE',  ( 8.466388902489056179, -58.63671300496882566, 1.826958383912698158 ) ) ;
#12954 = CARTESIAN_POINT ( 'NONE',  ( 29.69047892279255407, -53.28399145779480506, -4.141535524925019196 ) ) ;
#12955 = DIRECTION ( 'NONE',  ( -1.000000000000000000, -0.000000000000000000, -0.000000000000000000 ) ) ;
#12956 = CARTESIAN_POINT ( 'NONE',  ( 32.44735717182409473, -60.71989949371816664, -2.646748467233224211 ) ) ;
#12957 = CARTESIAN_POINT ( 'NONE',  ( 93.56770215592470663, 0.000000000000000000, 33.00000000000012790 ) ) ;
#12958 = FACE_OUTER_BOUND ( 'NONE', #7616, .T. ) ;
#12959 = FACE_OUTER_BOUND ( 'NONE', #13755, .T. ) ;
#12960 = AXIS2_PLACEMENT_3D ( 'NONE', #4199, #13521, #11354 ) ;
#12961 = CARTESIAN_POINT ( 'NONE',  ( -16.99999999999998579, -2.249290599286303927, 47.50000000000012079 ) ) ;
#12962 = AXIS2_PLACEMENT_3D ( 'NONE', #3109, #7813, #12273 ) ;
#12963 = ORIENTED_EDGE ( 'NONE', *, *, #349, .F. ) ;
#12964 = ADVANCED_FACE ( 'NONE', ( #3571 ), #5814, .T. ) ;
#12965 = EDGE_CURVE ( 'NONE', #3666, #9198, #10502, .T. ) ;
#12966 = APPLICATION_CONTEXT ( 'automotive_design' ) ;
#12967 = VECTOR ( 'NONE', #10919, 1000.000000000000000 ) ;
#12968 = ORIENTED_EDGE ( 'NONE', *, *, #1883, .T. ) ;
#12969 = DIRECTION ( 'NONE',  ( 0.7546336727145946943, 0.5961293309129324092, -0.2741493039031500656 ) ) ;
#12970 = DIRECTION ( 'NONE',  ( -1.000000000000000000, 0.000000000000000000, 0.000000000000000000 ) ) ;
#12971 = ORIENTED_EDGE ( 'NONE', *, *, #8668, .T. ) ;
#12972 = DIRECTION ( 'NONE',  ( 4.163336342344333240E-14, -2.515349040166368078E-14, 1.000000000000000000 ) ) ;
#12973 = LINE ( 'NONE', #2426, #9275 ) ;
#12974 = VECTOR ( 'NONE', #11413, 1000.000000000000000 ) ;
#12975 = AXIS2_PLACEMENT_3D ( 'NONE', #1639, #1711, #7719 ) ;
#12976 = CARTESIAN_POINT ( 'NONE',  ( 69.43927565506325550, -3.017240787745353980, 76.72358418092962040 ) ) ;
#12977 = CARTESIAN_POINT ( 'NONE',  ( 75.52271037289314393, -7.388871293676331220, 71.19766410831374515 ) ) ;
#12978 = DIRECTION ( 'NONE',  ( -0.000000000000000000, -0.000000000000000000, 1.000000000000000000 ) ) ;
#12979 = CARTESIAN_POINT ( 'NONE',  ( -25.40673215887140657, -6.684475985750503391, 48.01308457333527002 ) ) ;
#12980 = AXIS2_PLACEMENT_3D ( 'NONE', #1212, #8308, #5923 ) ;
#12981 = CARTESIAN_POINT ( 'NONE',  ( 9.982851463787662638, -60.49988549795173043, 2.962481358178291391 ) ) ;
#12982 = CLOSED_SHELL ( 'NONE', ( #262, #2709, #10920, #7445, #5471, #3583, #7815, #14761, #5793, #1432, #8790, #8240, #1548, #12091, #14308, #4317, #13926 ) ) ;
#12983 = CARTESIAN_POINT ( 'NONE',  ( 29.67025276671635936, -52.24929059928631148, 3.114169983390998375 ) ) ;
#12984 = AXIS2_PLACEMENT_3D ( 'NONE', #5027, #8418, #7177 ) ;
#12985 = ORIENTED_EDGE ( 'NONE', *, *, #8967, .T. ) ;
#12986 = LINE ( 'NONE', #12913, #13424 ) ;
#12987 = EDGE_LOOP ( 'NONE', ( #1448, #8331, #11114, #13027 ) ) ;
#12988 = CARTESIAN_POINT ( 'NONE',  ( 0.000000000000000000, 21.75070940071356418, 139.1143251403882459 ) ) ;
#12989 = ORIENTED_EDGE ( 'NONE', *, *, #11289, .F. ) ;
#12990 = ORIENTED_EDGE ( 'NONE', *, *, #5484, .F. ) ;
#12991 = DIRECTION ( 'NONE',  ( 1.156482317317870492E-16, -1.000000000000000000, 0.000000000000000000 ) ) ;
#12992 = ADVANCED_FACE ( 'NONE', ( #11949 ), #13084, .T. ) ;
#12993 = DIRECTION ( 'NONE',  ( 0.8746197071345573892, -0.4848096202550657430, 0.000000000000000000 ) ) ;
#12994 = AXIS2_PLACEMENT_3D ( 'NONE', #12160, #8332, #2554 ) ;
#12995 = CARTESIAN_POINT ( 'NONE',  ( 10.58727470799617087, -61.88944072237683258, -2.366779157396529332 ) ) ;
#12996 = EDGE_CURVE ( 'NONE', #3720, #10536, #4710, .T. ) ;
#12997 = VECTOR ( 'NONE', #2273, 1000.000000000000000 ) ;
#12998 = CARTESIAN_POINT ( 'NONE',  ( 9.586149153331275485, -54.40375996999062380, 3.226241354721975263 ) ) ;
#12999 = DIRECTION ( 'NONE',  ( 0.9111637130653279515, 0.4120445218577777902, 0.000000000000000000 ) ) ;
#13000 = CARTESIAN_POINT ( 'NONE',  ( 20.86173033120691045, -57.24929059928630437, 0.000000000000000000 ) ) ;
#13001 = DIRECTION ( 'NONE',  ( 0.000000000000000000, -1.000000000000000000, 0.000000000000000000 ) ) ;
#13002 = EDGE_CURVE ( 'NONE', #5593, #1184, #13119, .T. ) ;
#13003 = ORIENTED_EDGE ( 'NONE', *, *, #7106, .F. ) ;
#13004 = ORIENTED_EDGE ( 'NONE', *, *, #13643, .F. ) ;
#13005 = CARTESIAN_POINT ( 'NONE',  ( -30.80945343098651890, -5.389243620311580329, -57.50000000000012079 ) ) ;
#13006 = EDGE_LOOP ( 'NONE', ( #9950, #2584, #10835, #6758 ) ) ;
#13007 = ORIENTED_EDGE ( 'NONE', *, *, #5326, .F. ) ;
#13008 = FACE_OUTER_BOUND ( 'NONE', #9770, .T. ) ;
#13009 = VERTEX_POINT ( 'NONE', #11725 ) ;
#13010 = DIRECTION ( 'NONE',  ( -0.000000000000000000, -0.000000000000000000, 1.000000000000000000 ) ) ;
#13011 = DIRECTION ( 'NONE',  ( -0.000000000000000000, 0.000000000000000000, -1.000000000000000000 ) ) ;
#13012 = VERTEX_POINT ( 'NONE', #5971 ) ;
#13013 = EDGE_CURVE ( 'NONE', #5320, #14082, #6119, .T. ) ;
#13014 = EDGE_CURVE ( 'NONE', #6839, #7436, #4217, .T. ) ;
#13015 = DIRECTION ( 'NONE',  ( 0.8746197071345570562, -0.4848096202550662981, 0.000000000000000000 ) ) ;
#13016 = LINE ( 'NONE', #7004, #13086 ) ;
#13017 = VERTEX_POINT ( 'NONE', #10728 ) ;
#13018 = CARTESIAN_POINT ( 'NONE',  ( -25.99999999999998934, -2.249290599286303927, -58.00000000000012079 ) ) ;
#13019 = CARTESIAN_POINT ( 'NONE',  ( 65.92402464212069901, -2.249290599286309256, 39.50000000000012790 ) ) ;
#13020 = VERTEX_POINT ( 'NONE', #4882 ) ;
#13021 = CARTESIAN_POINT ( 'NONE',  ( 65.35437866493117554, -11.86302964528753634, 72.64181548138913058 ) ) ;
#13022 = ORIENTED_EDGE ( 'NONE', *, *, #11222, .T. ) ;
#13023 = CARTESIAN_POINT ( 'NONE',  ( 54.07385127050791596, 1.678372679529495981, 54.56811043785582882 ) ) ;
#13024 = FILL_AREA_STYLE_COLOUR ( '', #8998 ) ;
#13025 = AXIS2_PLACEMENT_3D ( 'NONE', #10025, #8861, #7638 ) ;
#13026 = ORIENTED_EDGE ( 'NONE', *, *, #6966, .F. ) ;
#13027 = ORIENTED_EDGE ( 'NONE', *, *, #13743, .T. ) ;
#13028 = CARTESIAN_POINT ( 'NONE',  ( 0.000000000000000000, 0.000000000000000000, 0.000000000000000000 ) ) ;
#13029 = CARTESIAN_POINT ( 'NONE',  ( -1.197457146693678531, -2.220571218158920779, 48.00000000000012079 ) ) ;
#13030 = DIRECTION ( 'NONE',  ( 0.000000000000000000, 0.000000000000000000, 1.000000000000000000 ) ) ;
#13031 = LINE ( 'NONE', #13107, #866 ) ;
#13032 = DIRECTION ( 'NONE',  ( 1.000000000000000000, 0.000000000000000000, 0.000000000000000000 ) ) ;
#13033 = DIRECTION ( 'NONE',  ( -0.000000000000000000, 1.000000000000000000, 0.000000000000000000 ) ) ;
#13034 = DIRECTION ( 'NONE',  ( -0.3020115420618266211, 0.1674077314120194226, -0.9384901064608612842 ) ) ;
#13035 = EDGE_CURVE ( 'NONE', #4172, #4443, #14271, .T. ) ;
#13036 = CARTESIAN_POINT ( 'NONE',  ( 33.59652235677629051, -57.16383106728765284, 1.814529264940141662 ) ) ;
#13037 = AXIS2_PLACEMENT_3D ( 'NONE', #12896, #2419, #36 ) ;
#13038 = CARTESIAN_POINT ( 'NONE',  ( 29.69047892279255052, -53.28399145779481216, -4.141535524925020084 ) ) ;
#13039 = ORIENTED_EDGE ( 'NONE', *, *, #12949, .T. ) ;
#13040 = LINE ( 'NONE', #116, #2702 ) ;
#13041 = ORIENTED_EDGE ( 'NONE', *, *, #8530, .T. ) ;
#13042 = CARTESIAN_POINT ( 'NONE',  ( -80.00000000000001421, -85.24929059928629727, -8.000000000000001776 ) ) ;
#13043 = CARTESIAN_POINT ( 'NONE',  ( 31.95882812935311179, -60.25800154558402255, -2.890242835725726600 ) ) ;
#13044 = DIRECTION ( 'NONE',  ( 0.000000000000000000, -1.000000000000000000, 0.000000000000000000 ) ) ;
#13045 = CARTESIAN_POINT ( 'NONE',  ( -16.99999999999998579, 7.750709400713696517, 38.00000000000012079 ) ) ;
#13046=STYLED_ITEM('',(#15244),#8947);
#13047 = CARTESIAN_POINT ( 'NONE',  ( 70.12209330904275362, -3.652447179931426646, 75.96062414490636172 ) ) ;
#13048 = CARTESIAN_POINT ( 'NONE',  ( 64.77204481361067678, -11.50071871444543881, 71.61353507035619259 ) ) ;
#13049 = EDGE_CURVE ( 'NONE', #9539, #10074, #10307, .T. ) ;
#13050 = EDGE_CURVE ( 'NONE', #11368, #12474, #14791, .T. ) ;
#13051 = CARTESIAN_POINT ( 'NONE',  ( -24.80190065418678458, -6.760980545838084943, 48.43121057161747700 ) ) ;
#13052 = AXIS2_PLACEMENT_3D ( 'NONE', #3879, #13343, #9820 ) ;
#13053 = CARTESIAN_POINT ( 'NONE',  ( 32.50130901777686177, -54.90141807276702934, 3.067753764789294291 ) ) ;
#13054 = VERTEX_POINT ( 'NONE', #1908 ) ;
#13055 = DIRECTION ( 'NONE',  ( -0.000000000000000000, 0.000000000000000000, -1.000000000000000000 ) ) ;
#13056 = UNCERTAINTY_MEASURE_WITH_UNIT (LENGTH_MEASURE( 1.000000000000000082E-05 ), #10177, 'distance_accuracy_value', 'NONE');
#13057 = VERTEX_POINT ( 'NONE', #4374 ) ;
#13058 = CARTESIAN_POINT ( 'NONE',  ( 37.23881781239525424, 21.75070940071315562, -33.00000000000012790 ) ) ;
#13059 = ORIENTED_EDGE ( 'NONE', *, *, #3292, .F. ) ;
#13060 = VERTEX_POINT ( 'NONE', #15151 ) ;
#13061 = VECTOR ( 'NONE', #5852, 1000.000000000000000 ) ;
#13062 = CARTESIAN_POINT ( 'NONE',  ( 66.24771997929842371, -11.54120404467442285, 76.19766410831375936 ) ) ;
#13063 =( BOUNDED_SURFACE ( )  B_SPLINE_SURFACE ( 3, 2, ( 
 ( #3596, #6988, #4678 ),
 ( #3880, #8230, #1647 ),
 ( #9821, #2807, #67 ),
 ( #14147, #12184, #5921 ) ),
 .UNSPECIFIED., .F., .F., .F. ) 
 B_SPLINE_SURFACE_WITH_KNOTS ( ( 4, 4 ),
 ( 3, 3 ),
 ( 0.000000000000000000, 0.001771943201165739230 ),
 ( 0.000000000000000000, 1.000000000000000000 ),
 .UNSPECIFIED. ) 
 GEOMETRIC_REPRESENTATION_ITEM ( )  RATIONAL_B_SPLINE_SURFACE ( (
 ( 1.000000000000000000, 0.8250833044923664428, 1.000000000000000000),
 ( 1.000000000000000000, 0.8269348987755780200, 1.000000000000000000),
 ( 1.000000000000000000, 0.8288551047899420654, 1.000000000000000000),
 ( 1.000000000000000000, 0.8308543624379425285, 1.000000000000000000) ) ) 
 REPRESENTATION_ITEM ( '' )  SURFACE ( )  );
#13064 = CIRCLE ( 'NONE', #2742, 3.999999999999999112 ) ;
#13065 = CARTESIAN_POINT ( 'NONE',  ( 12.06345512429583877, -63.57773214734889677, -2.964070158660714327 ) ) ;
#13066 = ORIENTED_EDGE ( 'NONE', *, *, #8220, .T. ) ;
#13067 = DIRECTION ( 'NONE',  ( 0.000000000000000000, 0.000000000000000000, 1.000000000000000000 ) ) ;
#13068 = AXIS2_PLACEMENT_3D ( 'NONE', #11183, #4328, #634 ) ;
#13069 = CIRCLE ( 'NONE', #4963, 7.924024642120691908 ) ;
#13070 = FACE_OUTER_BOUND ( 'NONE', #6015, .T. ) ;
#13071 = ORIENTED_EDGE ( 'NONE', *, *, #7055, .F. ) ;
#13072 = TOROIDAL_SURFACE ( 'NONE', #15036, 2.000000000000000000, 1.000000000000000000 ) ;
#13073 = ORIENTED_EDGE ( 'NONE', *, *, #13002, .T. ) ;
#13074 = CARTESIAN_POINT ( 'NONE',  ( 65.03656227622965957, -11.30130833895906406, 76.98918051064211454 ) ) ;
#13075 = ORIENTED_EDGE ( 'NONE', *, *, #4673, .T. ) ;
#13076 = CARTESIAN_POINT ( 'NONE',  ( 62.67308791069655882, 29.52935533987996664, -33.00000000000013500 ) ) ;
#13077 = EDGE_LOOP ( 'NONE', ( #8477, #14333, #6304, #546 ) ) ;
#13078 = CARTESIAN_POINT ( 'NONE',  ( 29.30348265400095542, -64.16417350152460131, 3.791131921651011538 ) ) ;
#13079 = VERTEX_POINT ( 'NONE', #4447 ) ;
#13080 = AXIS2_PLACEMENT_3D ( 'NONE', #4787, #2164, #5878 ) ;
#13081 = DIRECTION ( 'NONE',  ( -1.000000000000000000, -1.156482317317870492E-16, 0.000000000000000000 ) ) ;
#13082 = DIRECTION ( 'NONE',  ( -1.000000000000000000, 0.000000000000000000, 0.000000000000000000 ) ) ;
#13083 = ORIENTED_EDGE ( 'NONE', *, *, #13984, .T. ) ;
#13084 = TOROIDAL_SURFACE ( 'NONE', #4972, 3.694885682587998765, 0.5000000000000000000 ) ;
#13085 = EDGE_CURVE ( 'NONE', #11311, #13981, #3252, .T. ) ;
#13086 = VECTOR ( 'NONE', #14240, 1000.000000000000000 ) ;
#13087 = CARTESIAN_POINT ( 'NONE',  ( 93.56770215592470663, 0.000000000000000000, -33.00000000000012790 ) ) ;
#13088 = DIRECTION ( 'NONE',  ( 0.8420378618367728718, 0.5394184268574404584, 0.000000000000000000 ) ) ;
#13089 = ORIENTED_EDGE ( 'NONE', *, *, #5278, .T. ) ;
#13090 = PLANE ( 'NONE',  #1452 ) ;
#13091 = DIRECTION ( 'NONE',  ( 0.000000000000000000, 0.000000000000000000, 1.000000000000000000 ) ) ;
#13092 = CARTESIAN_POINT ( 'NONE',  ( 20.86173033120691045, -82.24929059928629727, 0.000000000000000000 ) ) ;
#13093 = ORIENTED_EDGE ( 'NONE', *, *, #112, .T. ) ;
#13094 = CIRCLE ( 'NONE', #8186, 11.46463184759105403 ) ;
#13095 = DIRECTION ( 'NONE',  ( 0.000000000000000000, 0.000000000000000000, -1.000000000000000000 ) ) ;
#13096 = AXIS2_PLACEMENT_3D ( 'NONE', #7296, #6008, #146 ) ;
#13097 = EDGE_CURVE ( 'NONE', #12316, #4627, #11523, .T. ) ;
#13098 = VECTOR ( 'NONE', #8183, 1000.000000000000000 ) ;
#13099 = EDGE_CURVE ( 'NONE', #13646, #3062, #10130, .T. ) ;
#13100 = EDGE_LOOP ( 'NONE', ( #8010, #5834, #14677, #12267 ) ) ;
#13101 = VECTOR ( 'NONE', #5529, 1000.000000000000000 ) ;
#13102 = DIRECTION ( 'NONE',  ( -0.000000000000000000, -0.000000000000000000, -1.000000000000000000 ) ) ;
#13103 = VERTEX_POINT ( 'NONE', #7846 ) ;
#13104 = CARTESIAN_POINT ( 'NONE',  ( -11.04362772831848716, -9.031687326780717839, -48.03392779025379156 ) ) ;
#13105 = LINE ( 'NONE', #2562, #10390 ) ;
#13106 = EDGE_CURVE ( 'NONE', #322, #3968, #11605, .T. ) ;
#13107 = CARTESIAN_POINT ( 'NONE',  ( -80.00000000000001421, -72.24929059928631148, 34.99999999999999289 ) ) ;
#13108 = AXIS2_PLACEMENT_3D ( 'NONE', #14201, #10582, #10505 ) ;
#13109 = CARTESIAN_POINT ( 'NONE',  ( 6.986309121235717789, -48.72433491191959831, 2.732636121739603130 ) ) ;
#13110 = VECTOR ( 'NONE', #4525, 1000.000000000000000 ) ;
#13111 = LINE ( 'NONE', #14261, #10273 ) ;
#13112 = DIRECTION ( 'NONE',  ( -0.8746197071345570562, 0.4848096202550665756, 0.000000000000000000 ) ) ;
#13113 = CIRCLE ( 'NONE', #5237, 4.000000000000003553 ) ;
#13114 = CARTESIAN_POINT ( 'NONE',  ( -24.95893038578871881, -6.453098109823664608, 47.50000000000011369 ) ) ;
#13115 = CARTESIAN_POINT ( 'NONE',  ( 29.92873905722243322, -53.28554919726588679, -4.056729053556589193 ) ) ;
#13116 = CARTESIAN_POINT ( 'NONE',  ( 67.21328690825529861, 25.52935533987996664, -21.00807340887166674 ) ) ;
#13117 = EDGE_LOOP ( 'NONE', ( #13477, #2987, #4912, #1569, #7500 ) ) ;
#13118 =( NAMED_UNIT ( * ) PLANE_ANGLE_UNIT ( ) SI_UNIT ( $, .RADIAN. ) );
#13119 = LINE ( 'NONE', #12899, #2525 ) ;
#13120 = AXIS2_PLACEMENT_3D ( 'NONE', #8966, #7589, #2043 ) ;
#13121 = LINE ( 'NONE', #9589, #10398 ) ;
#13122 = CYLINDRICAL_SURFACE ( 'NONE', #5103, 0.7892041907098262810 ) ;
#13123 = EDGE_CURVE ( 'NONE', #11609, #11588, #14557, .T. ) ;
#13124 = AXIS2_PLACEMENT_3D ( 'NONE', #14397, #10857, #10627 ) ;
#13125 = CARTESIAN_POINT ( 'NONE',  ( 69.43199442225004248, -3.120433192335155592, 76.80468318204789568 ) ) ;
#13126 = CARTESIAN_POINT ( 'NONE',  ( -8.779641963837230279, 13.70511383897430058, 48.50000000000012079 ) ) ;
#13127 = CARTESIAN_POINT ( 'NONE',  ( -32.80254285330626374, -2.278009980413909563, -48.00000000000012079 ) ) ;
#13128 = LINE ( 'NONE', #4891, #2724 ) ;
#13129 = CARTESIAN_POINT ( 'NONE',  ( 32.55554926572738594, -53.68459816487440861, 2.283893849732154369 ) ) ;
#13130 = ORIENTED_EDGE ( 'NONE', *, *, #14267, .T. ) ;
#13131 = DIRECTION ( 'NONE',  ( -0.000000000000000000, -1.000000000000000000, -0.000000000000000000 ) ) ;
#13132 = VERTEX_POINT ( 'NONE', #830 ) ;
#13133 = DIRECTION ( 'NONE',  ( 1.000000000000000000, 0.000000000000000000, 0.000000000000000000 ) ) ;
#13134 = ORIENTED_EDGE ( 'NONE', *, *, #14568, .T. ) ;
#13135 = VERTEX_POINT ( 'NONE', #907 ) ;
#13137 = ORIENTED_EDGE ( 'NONE', *, *, #3854, .F. ) ;
#13136 = CARTESIAN_POINT ( 'NONE',  ( 65.13162939936435691, -11.91918766645189898, 75.26674478960599401 ) ) ;
#13138 = FACE_OUTER_BOUND ( 'NONE', #15064, .T. ) ;
#13139 = ADVANCED_FACE ( 'NONE', ( #12538 ), #10227, .T. ) ;
#13140 = EDGE_CURVE ( 'NONE', #5503, #7793, #2512, .T. ) ;
#13141 = DIRECTION ( 'NONE',  ( 0.000000000000000000, -1.000000000000000000, 0.000000000000000000 ) ) ;
#13142 = CARTESIAN_POINT ( 'NONE',  ( 8.093541475047761224, -56.17545244456535869, 1.862977194133688341 ) ) ;
#13143 = EDGE_CURVE ( 'NONE', #15028, #14077, #13329, .T. ) ;
#13144 = CARTESIAN_POINT ( 'NONE',  ( -23.02941217286474185, 4.529839663208023559, 48.26891069786830002 ) ) ;
#13145 = DIRECTION ( 'NONE',  ( -0.000000000000000000, 0.000000000000000000, -1.000000000000000000 ) ) ;
#13146 = VERTEX_POINT ( 'NONE', #1983 ) ;
#13147 = ORIENTED_EDGE ( 'NONE', *, *, #6147, .T. ) ;
#13148 = LINE ( 'NONE', #2600, #9534 ) ;
#13149 = VERTEX_POINT ( 'NONE', #7768 ) ;
#13150 =( BOUNDED_SURFACE ( )  B_SPLINE_SURFACE ( 3, 2, ( 
 ( #14663, #13431, #2896 ),
 ( #12431, #7593, #4118 ),
 ( #8813, #12283, #1736 ),
 ( #13512, #6436, #1817 ),
 ( #13664, #10053, #10133 ),
 ( #3053, #4267, #6507 ) ),
 .UNSPECIFIED., .F., .F., .F. ) 
 B_SPLINE_SURFACE_WITH_KNOTS ( ( 4, 2, 4 ),
 ( 3, 3 ),
 ( -9.757819552369539906E-18, 0.001008510999900088731, 0.002017021999800187437 ),
 ( 0.000000000000000000, 1.000000000000000000 ),
 .UNSPECIFIED. ) 
 GEOMETRIC_REPRESENTATION_ITEM ( )  RATIONAL_B_SPLINE_SURFACE ( (
 ( 1.000000000000000000, 0.8053615646146047302, 1.000000000000000000),
 ( 1.000000000000000000, 0.8146689552415620206, 1.000000000000000000),
 ( 1.000000000000000000, 0.8215765256473256395, 1.000000000000000000),
 ( 1.000000000000000000, 0.8301698670440428307, 1.000000000000000000),
 ( 1.000000000000000000, 0.8316880482409466646, 1.000000000000000000),
 ( 1.000000000000000000, 0.8308543624379426396, 1.000000000000000000) ) ) 
 REPRESENTATION_ITEM ( '' )  SURFACE ( )  );
#13151 = DIRECTION ( 'NONE',  ( -1.000000000000000000, 9.251858538542971581E-17, -0.000000000000000000 ) ) ;
#13152 = ORIENTED_EDGE ( 'NONE', *, *, #6390, .T. ) ;
#13153 = CARTESIAN_POINT ( 'NONE',  ( 31.72322230991231962, -61.42570632716525125, 2.132522520905375973 ) ) ;
#13154 = ADVANCED_FACE ( 'NONE', ( #12454 ), #6757, .F. ) ;
#13155 = ORIENTED_EDGE ( 'NONE', *, *, #3453, .T. ) ;
#13156 = PLANE ( 'NONE',  #4077 ) ;
#13157 = CARTESIAN_POINT ( 'NONE',  ( -10.80198322015283097, -8.784136766666819085, 47.93908580834070676 ) ) ;
#13158 = ORIENTED_EDGE ( 'NONE', *, *, #12183, .F. ) ;
#13159 = DIRECTION ( 'NONE',  ( -0.000000000000000000, -0.000000000000000000, -1.000000000000000000 ) ) ;
#13160 = DIRECTION ( 'NONE',  ( 0.000000000000000000, -1.000000000000000000, 0.000000000000000000 ) ) ;
#13161 = ORIENTED_EDGE ( 'NONE', *, *, #3102, .T. ) ;
#13162 = LINE ( 'NONE', #7309, #13693 ) ;
#13163 = CARTESIAN_POINT ( 'NONE',  ( -24.12409601409935078, -6.885803942510236197, 58.00000000000012079 ) ) ;
#13164 = CYLINDRICAL_SURFACE ( 'NONE', #5998, 2.000000000000000000 ) ;
#13165 = ORIENTED_EDGE ( 'NONE', *, *, #5916, .T. ) ;
#13166 = DIRECTION ( 'NONE',  ( 0.000000000000000000, -1.000000000000000000, 0.000000000000000000 ) ) ;
#13167 = ORIENTED_EDGE ( 'NONE', *, *, #4717, .T. ) ;
#13168 = CARTESIAN_POINT ( 'NONE',  ( 59.31076468612580754, 2.638779099491020297, 62.84860122826521689 ) ) ;
#13169 = CARTESIAN_POINT ( 'NONE',  ( 27.55953187330915810, 0.000000000000000000, -33.00000000000012790 ) ) ;
#13170 = ORIENTED_EDGE ( 'NONE', *, *, #14400, .F. ) ;
#13171 = PRODUCT_CONTEXT ( 'NONE', #9533, 'mechanical' ) ;
#13172 = FACE_OUTER_BOUND ( 'NONE', #5307, .T. ) ;
#13173 = EDGE_CURVE ( 'NONE', #8468, #14864, #4290, .T. ) ;
#13174 = CARTESIAN_POINT ( 'NONE',  ( 27.60448374887417344, -53.27035328036003392, -4.884026039770254179 ) ) ;
#13175 = CARTESIAN_POINT ( 'NONE',  ( -9.391954890838034586, 2.559027098228045638, -47.99579695943414492 ) ) ;
#13176 = VECTOR ( 'NONE', #8415, 1000.000000000000000 ) ;
#13177 = DIRECTION ( 'NONE',  ( 1.000000000000000000, 1.156482317317870492E-16, 0.000000000000000000 ) ) ;
#13178 = EDGE_CURVE ( 'NONE', #7204, #8564, #6837, .T. ) ;
#13179 = EDGE_CURVE ( 'NONE', #6910, #6609, #6916, .T. ) ;
#13180 = CARTESIAN_POINT ( 'NONE',  ( 118.0000000000000284, 19.25070940071370273, -33.00000000000012790 ) ) ;
#13181 = CARTESIAN_POINT ( 'NONE',  ( 56.56161818778031858, -7.613266777470379942, 60.61639468829817190 ) ) ;
#13182 = CARTESIAN_POINT ( 'NONE',  ( -24.78493442214762155, -6.766828585132234508, 47.63220435834860922 ) ) ;
#13183 = CARTESIAN_POINT ( 'NONE',  ( 30.88646442064404241, -52.52046121080019248, -2.777687341764009332 ) ) ;
#13184 = EDGE_CURVE ( 'NONE', #9911, #7757, #6446, .T. ) ;
#13185 = AXIS2_PLACEMENT_3D ( 'NONE', #6627, #11312, #10178 ) ;
#13186 = FACE_OUTER_BOUND ( 'NONE', #2897, .T. ) ;
#13187 = VERTEX_POINT ( 'NONE', #13764 ) ;
#13188 = CARTESIAN_POINT ( 'NONE',  ( 80.00000000000001421, -72.24929059928631148, -34.99999999999999289 ) ) ;
#13189 = CARTESIAN_POINT ( 'NONE',  ( 37.23881781239525424, 23.25070940071368852, 139.1143251403882459 ) ) ;
#13190 = ORIENTED_EDGE ( 'NONE', *, *, #7814, .F. ) ;
#13191 = DIRECTION ( 'NONE',  ( 0.000000000000000000, -0.000000000000000000, -1.000000000000000000 ) ) ;
#13192 = ORIENTED_EDGE ( 'NONE', *, *, #3576, .T. ) ;
#13193 = EDGE_CURVE ( 'NONE', #505, #10236, #754, .T. ) ;
#13194 = CARTESIAN_POINT ( 'NONE',  ( 70.07305199753827196, -3.471083832564866967, 75.82119617954428747 ) ) ;
#13195 = CARTESIAN_POINT ( 'NONE',  ( 40.00000000000002132, -74.24929059928642516, 32.99999999999999289 ) ) ;
#13196 = CIRCLE ( 'NONE', #2854, 1.000000000000001998 ) ;
#13197 = EDGE_CURVE ( 'NONE', #4927, #11787, #2068, .T. ) ;
#13198 = VECTOR ( 'NONE', #2738, 1000.000000000000000 ) ;
#13199 = FACE_OUTER_BOUND ( 'NONE', #14723, .T. ) ;
#13200 = DIRECTION ( 'NONE',  ( 0.000000000000000000, 0.000000000000000000, 1.000000000000000000 ) ) ;
#13201 = AXIS2_PLACEMENT_3D ( 'NONE', #13005, #14229, #6155 ) ;
#13202 = EDGE_CURVE ( 'NONE', #4172, #3738, #9388, .T. ) ;
#13203 = CARTESIAN_POINT ( 'NONE',  ( 18.61871093201827065, -53.24929059928630437, -5.564967562786291566 ) ) ;
#13204 = EDGE_CURVE ( 'NONE', #11349, #3333, #8313, .T. ) ;
#13205 = VERTEX_POINT ( 'NONE', #9620 ) ;
#13206 = FACE_BOUND ( 'NONE', #12638, .T. ) ;
#13207 = UNCERTAINTY_MEASURE_WITH_UNIT (LENGTH_MEASURE( 1.000000000000000082E-05 ), #6778, 'distance_accuracy_value', 'NONE');
#13208 = ORIENTED_EDGE ( 'NONE', *, *, #1529, .F. ) ;
#13209 = FACE_OUTER_BOUND ( 'NONE', #13869, .T. ) ;
#13210 = VECTOR ( 'NONE', #2801, 1000.000000000000000 ) ;
#13211 = EDGE_LOOP ( 'NONE', ( #3552, #10270, #5457, #12210 ) ) ;
#13213 = ORIENTED_EDGE ( 'NONE', *, *, #14361, .T. ) ;
#13212 = FACE_OUTER_BOUND ( 'NONE', #6247, .T. ) ;
#13214 = FACE_OUTER_BOUND ( 'NONE', #15175, .T. ) ;
#13215 = DIRECTION ( 'NONE',  ( 1.000000000000000000, 0.000000000000000000, 0.000000000000000000 ) ) ;
#13216 = ADVANCED_FACE ( 'NONE', ( #13008 ), #1136, .F. ) ;
#13217 = AXIS2_PLACEMENT_3D ( 'NONE', #13203, #9597, #8364 ) ;
#13218 = ORIENTED_EDGE ( 'NONE', *, *, #13179, .T. ) ;
#13219 = CARTESIAN_POINT ( 'NONE',  ( 8.599038152243162259, -54.47420853489223447, 2.874994438546353503 ) ) ;
#13220 = AXIS2_PLACEMENT_3D ( 'NONE', #1699, #1196, #5097 ) ;
#13221 = LINE ( 'NONE', #14451, #3276 ) ;
#13222 = ADVANCED_FACE ( 'NONE', ( #8383 ), #1775, .T. ) ;
#13223 = ADVANCED_FACE ( 'NONE', ( #3682 ), #7074, .F. ) ;
#13224 = DIRECTION ( 'NONE',  ( -0.000000000000000000, -0.000000000000000000, 1.000000000000000000 ) ) ;
#13225 = ORIENTED_EDGE ( 'NONE', *, *, #5053, .F. ) ;
#13226 = ORIENTED_EDGE ( 'NONE', *, *, #13362, .F. ) ;
#13227 = DIRECTION ( 'NONE',  ( -0.000000000000000000, -0.000000000000000000, -1.000000000000000000 ) ) ;
#13228 = B_SPLINE_CURVE_WITH_KNOTS ( 'NONE', 3,
 ( #13475, #4229, #764, #1703 ),
 .UNSPECIFIED., .F., .F.,
 ( 4, 4 ),
 ( 0.000000000000000000, 0.003645914952990592789 ),
 .UNSPECIFIED. ) ;
#13229 = VERTEX_POINT ( 'NONE', #3755 ) ;
#13230 = ORIENTED_EDGE ( 'NONE', *, *, #13700, .T. ) ;
#13231 = FACE_OUTER_BOUND ( 'NONE', #1009, .T. ) ;
#13232 = AXIS2_PLACEMENT_3D ( 'NONE', #7163, #10940, #5013 ) ;
#13233 = ORIENTED_EDGE ( 'NONE', *, *, #8381, .T. ) ;
#13234 = CARTESIAN_POINT ( 'NONE',  ( 29.87892709566704497, -63.30956378473970148, 2.875213255997512540 ) ) ;
#13235 = ORIENTED_EDGE ( 'NONE', *, *, #2460, .T. ) ;
#13236 = CIRCLE ( 'NONE', #14935, 8.924024642120691908 ) ;
#13237 = CARTESIAN_POINT ( 'NONE',  ( 65.00000000000001421, -87.24929059928631148, -22.49999999999999289 ) ) ;
#13238 = DIRECTION ( 'NONE',  ( -0.000000000000000000, 1.000000000000000000, -0.000000000000000000 ) ) ;
#13239 = EDGE_LOOP ( 'NONE', ( #2757, #10633, #7524, #13727 ) ) ;
#13240 =( REPRESENTATION_RELATIONSHIP ('NONE','NONE', #15125, #2449 ) REPRESENTATION_RELATIONSHIP_WITH_TRANSFORMATION ( #5386 )SHAPE_REPRESENTATION_RELATIONSHIP( ) );
#13241 = CARTESIAN_POINT ( 'NONE',  ( -80.00000000000001421, -74.24929059928631148, 32.00000000000000000 ) ) ;
#13242 = DIRECTION ( 'NONE',  ( 0.000000000000000000, 0.000000000000000000, -1.000000000000000000 ) ) ;
#13243 = ORIENTED_EDGE ( 'NONE', *, *, #3896, .T. ) ;
#13244 = EDGE_CURVE ( 'NONE', #9663, #8444, #7843, .T. ) ;
#13245 = CARTESIAN_POINT ( 'NONE',  ( 48.84742675818896629, 2.824063592853379046, 60.61639468829817190 ) ) ;
#13246 = CARTESIAN_POINT ( 'NONE',  ( -21.66581936427349575, -2.249290599286304371, -50.00000000000012079 ) ) ;
#13247 = ADVANCED_FACE ( 'NONE', ( #3605 ), #226, .F. ) ;
#13248 = CARTESIAN_POINT ( 'NONE',  ( 40.33162949095117966, 21.75070940071319114, 139.1143251403882459 ) ) ;
#13249 = ORIENTED_EDGE ( 'NONE', *, *, #9895, .F. ) ;
#13250 = CARTESIAN_POINT ( 'NONE',  ( -23.87164973098472487, 3.842474614898954144, 48.12459668492483189 ) ) ;
#13251 = VERTEX_POINT ( 'NONE', #14304 ) ;
#13252 = DIRECTION ( 'NONE',  ( 1.734723475976807292E-15, -1.000000000000000000, 0.000000000000000000 ) ) ;
#13253 = ORIENTED_EDGE ( 'NONE', *, *, #10832, .F. ) ;
#13254 = CARTESIAN_POINT ( 'NONE',  ( 56.59738969056744651, 21.75070940071329417, 33.00000000000012790 ) ) ;
#13255 = CARTESIAN_POINT ( 'NONE',  ( 56.13062797998802722, -6.952138427283281352, 48.51982618741349285 ) ) ;
#13256 = DIRECTION ( 'NONE',  ( 0.000000000000000000, 0.000000000000000000, 1.000000000000000000 ) ) ;
#13257 = CARTESIAN_POINT ( 'NONE',  ( 31.89675648641932071, -61.28862151863886965, 2.085432713781510738 ) ) ;
#13258 = CARTESIAN_POINT ( 'NONE',  ( -9.456839514482961562, 2.659958822950721835, 57.50000000000012079 ) ) ;
#13259 = CARTESIAN_POINT ( 'NONE',  ( 96.29968967959054282, 23.25070940071369208, 33.00000000000012790 ) ) ;
#13260 = CARTESIAN_POINT ( 'NONE',  ( 31.18383636339185827, -53.65556550047445228, -3.599583915703545411 ) ) ;
#13261 = AXIS2_PLACEMENT_3D ( 'NONE', #8770, #14414, #12018 ) ;
#13262 = VECTOR ( 'NONE', #2178, 1000.000000000000000 ) ;
#13263 = FACE_OUTER_BOUND ( 'NONE', #5642, .T. ) ;
#13264 = ORIENTED_EDGE ( 'NONE', *, *, #14571, .T. ) ;
#13265 = DIRECTION ( 'NONE',  ( -0.000000000000000000, -0.000000000000000000, -1.000000000000000000 ) ) ;
#13266 = LINE ( 'NONE', #5034, #9594 ) ;
#13267 = CARTESIAN_POINT ( 'NONE',  ( -30.80945343098651890, -5.389243620311580329, 57.50000000000012079 ) ) ;
#13268 = CARTESIAN_POINT ( 'NONE',  ( 8.821484763567294607, -57.33450387999030795, -2.749014434309871469 ) ) ;
#13269 = EDGE_CURVE ( 'NONE', #791, #4250, #8467, .T. ) ;
#13270 = CARTESIAN_POINT ( 'NONE',  ( 70.04298944718500763, -3.369224104032832567, 75.71372953216713597 ) ) ;
#13271 = DIRECTION ( 'NONE',  ( 0.000000000000000000, -1.000000000000000000, 0.000000000000000000 ) ) ;
#13272 = EDGE_CURVE ( 'NONE', #13625, #12856, #14287, .T. ) ;
#13273 = CIRCLE ( 'NONE', #6150, 4.000000000000003553 ) ;
#13274 = ADVANCED_FACE ( 'NONE', ( #12930 ), #11984, .T. ) ;
#13275 = CIRCLE ( 'NONE', #8594, 0.9999999999999954481 ) ;
#13276 = CARTESIAN_POINT ( 'NONE',  ( 80.00000000000001421, -76.24929059928631148, -4.000000000000000000 ) ) ;
#13277 = FACE_OUTER_BOUND ( 'NONE', #13860, .T. ) ;
#13278 = EDGE_LOOP ( 'NONE', ( #12597, #766, #1216, #11441 ) ) ;
#13279 = CARTESIAN_POINT ( 'NONE',  ( 28.78915391981847804, -54.56989982938152650, -4.214561585076694428 ) ) ;
#13280 = ORIENTED_EDGE ( 'NONE', *, *, #1328, .F. ) ;
#13281 = EDGE_CURVE ( 'NONE', #10908, #2336, #11135, .T. ) ;
#13282 = CARTESIAN_POINT ( 'NONE',  ( -30.80945343098651890, -5.389243620311580329, -48.50000000000012079 ) ) ;
#13283 = LINE ( 'NONE', #5192, #542 ) ;
#13284 = EDGE_CURVE ( 'NONE', #3110, #2589, #7674, .T. ) ;
#13285 = ORIENTED_EDGE ( 'NONE', *, *, #4021, .F. ) ;
#13286 = CARTESIAN_POINT ( 'NONE',  ( 80.00000000000001421, -74.24929059928631148, 32.00000000000000000 ) ) ;
#13287 = DIRECTION ( 'NONE',  ( 0.9274945937977119303, -6.485030681406579288E-16, 0.3738365665314423159 ) ) ;
#13288 = DIRECTION ( 'NONE',  ( 0.000000000000000000, 1.734723475976817547E-15, -1.000000000000000000 ) ) ;
#13289 = ORIENTED_EDGE ( 'NONE', *, *, #3385, .T. ) ;
#13290 = CARTESIAN_POINT ( 'NONE',  ( 53.41380296247595538, -0.1096349785133995947, 60.61639468829817190 ) ) ;
#13291 = DIRECTION ( 'NONE',  ( -0.2245701561649801337, 0.9744137433416110161, 0.009279102705852840596 ) ) ;
#13292 = ORIENTED_EDGE ( 'NONE', *, *, #11766, .F. ) ;
#13293 = ORIENTED_EDGE ( 'NONE', *, *, #13984, .F. ) ;
#13294 = DIRECTION ( 'NONE',  ( 0.000000000000000000, -0.000000000000000000, 1.000000000000000000 ) ) ;
#13295 = ORIENTED_EDGE ( 'NONE', *, *, #11517, .T. ) ;
#13296 = CARTESIAN_POINT ( 'NONE',  ( -24.72817752516938228, 2.363221963240404566, 47.50000000000012079 ) ) ;
#13297 = ORIENTED_EDGE ( 'NONE', *, *, #11516, .T. ) ;
#13298 = CARTESIAN_POINT ( 'NONE',  ( 31.27094208184040625, -61.76394201827576325, 3.065891788227224080 ) ) ;
#13299 = AXIS2_PLACEMENT_3D ( 'NONE', #8124, #4580, #2429 ) ;
#13300 = EDGE_LOOP ( 'NONE', ( #7812, #9214, #5625, #8819 ) ) ;
#13301 = PLANE ( 'NONE',  #8788 ) ;
#13302 = DIRECTION ( 'NONE',  ( -0.000000000000000000, 1.000000000000000000, -0.000000000000000000 ) ) ;
#13303 = ORIENTED_EDGE ( 'NONE', *, *, #12947, .F. ) ;
#13304 = ADVANCED_FACE ( 'NONE', ( #11131 ), #13434, .T. ) ;
#13305 = DIRECTION ( 'NONE',  ( -0.000000000000000000, -0.000000000000000000, 1.000000000000000000 ) ) ;
#13306 = AXIS2_PLACEMENT_3D ( 'NONE', #4121, #6509, #8817 ) ;
#13307 = VERTEX_POINT ( 'NONE', #6438 ) ;
#13308 = VECTOR ( 'NONE', #11555, 1000.000000000000000 ) ;
#13309 = CARTESIAN_POINT ( 'NONE',  ( 61.44362764059101067, -6.606194471396438672, 54.56811043785582882 ) ) ;
#13310 = DIRECTION ( 'NONE',  ( -0.000000000000000000, 0.000000000000000000, -1.000000000000000000 ) ) ;
#13311 = CARTESIAN_POINT ( 'NONE',  ( -65.00000000000001421, -85.24929059928631148, 22.49999999999999289 ) ) ;
#13312 = ORIENTED_EDGE ( 'NONE', *, *, #2868, .T. ) ;
#13313 = CARTESIAN_POINT ( 'NONE',  ( -23.72465974793126620, 3.743354278179100714, 47.97348817130775700 ) ) ;
#13314 = EDGE_LOOP ( 'NONE', ( #12553, #14391, #14649, #3374, #1440, #11365, #3057, #2588, #12040 ) ) ;
#13315 = VECTOR ( 'NONE', #10821, 1000.000000000000000 ) ;
#13316 = ORIENTED_EDGE ( 'NONE', *, *, #4119, .F. ) ;
#13317 = VECTOR ( 'NONE', #9779, 1000.000000000000000 ) ;
#13318 = DIRECTION ( 'NONE',  ( 0.000000000000000000, 0.000000000000000000, 1.000000000000000000 ) ) ;
#13319 = ORIENTED_EDGE ( 'NONE', *, *, #5455, .F. ) ;
#13320 = VECTOR ( 'NONE', #14318, 1000.000000000000000 ) ;
#13321 = PRODUCT_CONTEXT ( 'NONE', #3220, 'mechanical' ) ;
#13322 = DIRECTION ( 'NONE',  ( 0.000000000000000000, 1.000000000000000000, 0.000000000000000000 ) ) ;
#13323 = CARTESIAN_POINT ( 'NONE',  ( -16.99999999999998579, -2.249290599286303927, 57.50000000000012079 ) ) ;
#13324 = ADVANCED_FACE ( 'NONE', ( #2825 ), #9982, .F. ) ;
#13325 = DIRECTION ( 'NONE',  ( 0.000000000000000000, 0.000000000000000000, 1.000000000000000000 ) ) ;
#13326 = DIRECTION ( 'NONE',  ( 0.000000000000000000, -0.000000000000000000, -1.000000000000000000 ) ) ;
#13327 = CIRCLE ( 'NONE', #9883, 3.694885682588112896 ) ;
#13328 = CARTESIAN_POINT ( 'NONE',  ( 62.30678795759143185, -4.906903613034745426, 62.84860122826521689 ) ) ;
#13329 = CIRCLE ( 'NONE', #8651, 2.500000000000002220 ) ;
#13330 = DIRECTION ( 'NONE',  ( 1.000000000000000000, 0.000000000000000000, 0.000000000000000000 ) ) ;
#13331 = CARTESIAN_POINT ( 'NONE',  ( 13.51972775594646770, -66.75404937493283342, -3.551013195542459311 ) ) ;
#13332 = AXIS2_PLACEMENT_3D ( 'NONE', #11158, #14616, #2928 ) ;
#13333 = AXIS2_PLACEMENT_3D ( 'NONE', #4691, #9393, #10617 ) ;
#13334 = CARTESIAN_POINT ( 'NONE',  ( 114.6731053250840233, 0.000000000000000000, 13.14990448602693007 ) ) ;
#13335 = ORIENTED_EDGE ( 'NONE', *, *, #12418, .F. ) ;
#13336 = FILL_AREA_STYLE ('',( #3866 ) ) ;
#13337 = DIRECTION ( 'NONE',  ( -0.5394184268574414576, 0.8420378618367722057, 0.000000000000000000 ) ) ;
#13338 = EDGE_CURVE ( 'NONE', #2898, #13205, #6192, .T. ) ;
#13339 = CARTESIAN_POINT ( 'NONE',  ( 8.948125790170781357, -57.91121052158847959, -2.751677492798585423 ) ) ;
#13340 = CARTESIAN_POINT ( 'NONE',  ( 33.38971411695204949, -58.06117555224668081, -1.821720187976995975 ) ) ;
#13341 = CARTESIAN_POINT ( 'NONE',  ( 65.71319926014255941, -10.73129157630437547, 71.19766410831374515 ) ) ;
#13342 = VECTOR ( 'NONE', #14486, 1000.000000000000000 ) ;
#13343 = DIRECTION ( 'NONE',  ( 0.000000000000000000, 0.000000000000000000, -1.000000000000000000 ) ) ;
#13344 = DIRECTION ( 'NONE',  ( 0.000000000000000000, 1.000000000000000000, -0.000000000000000000 ) ) ;
#13345 = EDGE_CURVE ( 'NONE', #4156, #3899, #2979, .T. ) ;
#13346 = ORIENTED_EDGE ( 'NONE', *, *, #10701, .F. ) ;
#13347 = AXIS2_PLACEMENT_3D ( 'NONE', #10534, #12684, #2370 ) ;
#13348 = DIRECTION ( 'NONE',  ( -0.000000000000000000, 0.000000000000000000, -1.000000000000000000 ) ) ;
#13349 = EDGE_LOOP ( 'NONE', ( #12238, #10700 ) ) ;
#13350 = LINE ( 'NONE', #7503, #3486 ) ;
#13351 = PLANE ( 'NONE',  #5450 ) ;
#13352 = ORIENTED_EDGE ( 'NONE', *, *, #10420, .T. ) ;
#13354 = VERTEX_POINT ( 'NONE', #8599 ) ;
#13353 = CARTESIAN_POINT ( 'NONE',  ( -16.99999999999998579, -2.249290599286303927, 33.00000000000012790 ) ) ;
#13355 = FACE_OUTER_BOUND ( 'NONE', #4583, .T. ) ;
#13356 = CARTESIAN_POINT ( 'NONE',  ( 108.0866310645538562, 21.75070940071366365, 33.00000000000012790 ) ) ;
#13357 = EDGE_CURVE ( 'NONE', #143, #2517, #15055, .T. ) ;
#13358 = EDGE_LOOP ( 'NONE', ( #11965, #5075, #2189, #13161 ) ) ;
#13359 = CARTESIAN_POINT ( 'NONE',  ( 10.83699624176960619, -52.52046121080027774, 2.777687341763831697 ) ) ;
#13360 = EDGE_CURVE ( 'NONE', #14177, #15000, #1530, .T. ) ;
#13361 = VECTOR ( 'NONE', #10930, 1000.000000000000000 ) ;
#13362 = EDGE_CURVE ( 'NONE', #11787, #2219, #9632, .T. ) ;
#13363 = EDGE_CURVE ( 'NONE', #10236, #1125, #13892, .T. ) ;
#13364 = DIRECTION ( 'NONE',  ( 0.000000000000000000, 1.000000000000000000, -0.000000000000000000 ) ) ;
#13365 = DIRECTION ( 'NONE',  ( -0.000000000000000000, 1.000000000000000000, 0.000000000000000000 ) ) ;
#13366 = EDGE_LOOP ( 'NONE', ( #5080, #2353, #5094, #10004 ) ) ;
#13367 = CARTESIAN_POINT ( 'NONE',  ( 40.00000000000002132, -72.24929059928631148, 33.00000000000000000 ) ) ;
#13368 = ORIENTED_EDGE ( 'NONE', *, *, #11525, .F. ) ;
#13369 = ADVANCED_FACE ( 'NONE', ( #13231 ), #12345, .T. ) ;
#13370 = EDGE_LOOP ( 'NONE', ( #4188, #14158, #5546, #10055 ) ) ;
#13371 = FACE_OUTER_BOUND ( 'NONE', #9624, .T. ) ;
#13372 = ORIENTED_EDGE ( 'NONE', *, *, #2739, .T. ) ;
#13373 = DIRECTION ( 'NONE',  ( 8.673617379884035472E-17, -1.000000000000000000, 0.000000000000000000 ) ) ;
#13374 = CYLINDRICAL_SURFACE ( 'NONE', #10670, 0.7892041907098262810 ) ;
#13375 = ORIENTED_EDGE ( 'NONE', *, *, #4991, .T. ) ;
#13376 = CARTESIAN_POINT ( 'NONE',  ( 31.88156390563088749, -61.30062302791112927, -2.840369378987770421 ) ) ;
#13377 = ORIENTED_EDGE ( 'NONE', *, *, #9328, .T. ) ;
#13378 = CARTESIAN_POINT ( 'NONE',  ( 61.44362764059101067, -6.606194471396438672, 60.61639468829817190 ) ) ;
#13379 = LINE ( 'NONE', #7610, #4943 ) ;
#13380 = LINE ( 'NONE', #7689, #12878 ) ;
#13381 = ORIENTED_EDGE ( 'NONE', *, *, #2503, .T. ) ;
#13382 = CARTESIAN_POINT ( 'NONE',  ( 0.000000000000000000, 21.75070940071363168, 139.1143251403882459 ) ) ;
#13383 = VERTEX_POINT ( 'NONE', #14458 ) ;
#13384 = ORIENTED_EDGE ( 'NONE', *, *, #6088, .F. ) ;
#13385 = CARTESIAN_POINT ( 'NONE',  ( 31.89712467290438269, -61.28833066657261952, -2.085332803602909291 ) ) ;
#13386 = ITEM_DEFINED_TRANSFORMATION ( 'NONE', 'NONE', #7795,  #6315 ) ;
#13387 = DIRECTION ( 'NONE',  ( 0.000000000000000000, 0.000000000000000000, 1.000000000000000000 ) ) ;
#13388 = DIRECTION ( 'NONE',  ( -0.000000000000000000, -0.000000000000000000, -1.000000000000000000 ) ) ;
#13389 = CARTESIAN_POINT ( 'NONE',  ( -16.99999999999998579, -6.754727345143736628, 36.00000000000012079 ) ) ;
#13390 = CARTESIAN_POINT ( 'NONE',  ( 18.24879706501207721, -53.10810670090265262, 6.494041865157049287 ) ) ;
#13391 = DIRECTION ( 'NONE',  ( 0.000000000000000000, 1.000000000000000000, 1.734723475976817547E-15 ) ) ;
#13392 = CARTESIAN_POINT ( 'NONE',  ( -9.090012166261184134, -7.380334305945262408, -48.00000000000014211 ) ) ;
#13393 = CARTESIAN_POINT ( 'NONE',  ( -24.54316048551696028, -7.158540021523408292, 48.50000000000012079 ) ) ;
#13394 = DIRECTION ( 'NONE',  ( 1.000000000000000000, 0.000000000000000000, 0.000000000000000000 ) ) ;
#13395 = ADVANCED_FACE ( 'NONE', ( #12145 ), #2679, .F. ) ;
#13396 = ADVANCED_FACE ( 'NONE', ( #1599 ), #9844, .T. ) ;
#13397 = CARTESIAN_POINT ( 'NONE',  ( 68.00000000000001421, -2.249290599286293268, -33.00000000000012790 ) ) ;
#13398 = ORIENTED_EDGE ( 'NONE', *, *, #6195, .T. ) ;
#13399 = PRESENTATION_STYLE_ASSIGNMENT (( #14563 ) ) ;
#13400 = FACE_OUTER_BOUND ( 'NONE', #2005, .T. ) ;
#13401 = AXIS2_PLACEMENT_3D ( 'NONE', #6554, #10030, #14790 ) ;
#13402 =( NAMED_UNIT ( * ) PLANE_ANGLE_UNIT ( ) SI_UNIT ( $, .RADIAN. ) );
#13403 = DIRECTION ( 'NONE',  ( -0.000000000000000000, -0.000000000000000000, -1.000000000000000000 ) ) ;
#13404 = CARTESIAN_POINT ( 'NONE',  ( 9.834282440617473142, -54.14192065903538520, 3.328125142887254029 ) ) ;
#13405 = DIRECTION ( 'NONE',  ( -0.000000000000000000, -1.000000000000000000, -0.000000000000000000 ) ) ;
#13406 = DIRECTION ( 'NONE',  ( -0.000000000000000000, -0.000000000000000000, -1.000000000000000000 ) ) ;
#13407 = CARTESIAN_POINT ( 'NONE',  ( -24.79038709231510040, -6.757381419356298657, -47.62582736825572738 ) ) ;
#13408 = EDGE_CURVE ( 'NONE', #3440, #14689, #2339, .T. ) ;
#13409 = EDGE_CURVE ( 'NONE', #7882, #5809, #7410, .T. ) ;
#13410 = PRODUCT_RELATED_PRODUCT_CATEGORY ( 'part', '', ( #5935 ) ) ;
#13411 = VERTEX_POINT ( 'NONE', #10291 ) ;
#13412 = CARTESIAN_POINT ( 'NONE',  ( 17.09549820959326638, -85.24929059928631148, -1.347403282660980528 ) ) ;
#13413 = EDGE_LOOP ( 'NONE', ( #7101, #8481, #6311, #9789 ) ) ;
#13414 = CARTESIAN_POINT ( 'NONE',  ( -80.00000000000001421, -76.24929059928631148, -6.000000000000000000 ) ) ;
#13415 = CYLINDRICAL_SURFACE ( 'NONE', #12583, 0.7892041907098262810 ) ;
#13416 = ORIENTED_EDGE ( 'NONE', *, *, #13485, .T. ) ;
#13417 = CARTESIAN_POINT ( 'NONE',  ( 100.1541764164548880, 21.75070940071359615, 139.1143251403882459 ) ) ;
#13418 = CARTESIAN_POINT ( 'NONE',  ( 13.92166289842272597, -69.39711819508849544, -3.972674503026252246 ) ) ;
#13419 = CIRCLE ( 'NONE', #14894, 10.00000000000000000 ) ;
#13420 = AXIS2_PLACEMENT_3D ( 'NONE', #12193, #11043, #9829 ) ;
#13421 = DIRECTION ( 'NONE',  ( 0.000000000000000000, -1.000000000000000000, -1.734723475976817547E-15 ) ) ;
#13422 = ORIENTED_EDGE ( 'NONE', *, *, #10584, .T. ) ;
#13423 = CARTESIAN_POINT ( 'NONE',  ( 10.12753145436369451, -53.91129217357575953, 3.442845340291940559 ) ) ;
#13424 = VECTOR ( 'NONE', #3806, 1000.000000000000000 ) ;
#13425 = CARTESIAN_POINT ( 'NONE',  ( 14.38963276113423895, -69.39711819508849544, 4.502057496415707405 ) ) ;
#13426 = CARTESIAN_POINT ( 'NONE',  ( -25.15752072101212278, 2.619472661158555038, -48.00000000000012079 ) ) ;
#13427 = AXIS2_PLACEMENT_3D ( 'NONE', #3060, #14899, #3206 ) ;
#13428 = ORIENTED_EDGE ( 'NONE', *, *, #8091, .F. ) ;
#13429 = ORIENTED_EDGE ( 'NONE', *, *, #12088, .T. ) ;
#13430 = CIRCLE ( 'NONE', #4857, 4.000000000000003553 ) ;
#13431 = CARTESIAN_POINT ( 'NONE',  ( 9.841896756782944067, -61.30062302791112927, 2.840369378987773530 ) ) ;
#13432 = EDGE_CURVE ( 'NONE', #777, #7803, #11571, .T. ) ;
#13433 = ORIENTED_EDGE ( 'NONE', *, *, #7357, .F. ) ;
#13434 = PLANE ( 'NONE',  #3746 ) ;
#13435 = EDGE_LOOP ( 'NONE', ( #9627, #2675, #8219, #3589 ) ) ;
#13436 = CARTESIAN_POINT ( 'NONE',  ( 27.67989258697498300, -66.53205946168893092, 4.446982897616673647 ) ) ;
#13437 = FACE_OUTER_BOUND ( 'NONE', #6137, .T. ) ;
#13438 = APPLICATION_CONTEXT ( 'automotive_design' ) ;
#13439 = AXIS2_PLACEMENT_3D ( 'NONE', #13762, #8072, #6914 ) ;
#13440 = ORIENTED_EDGE ( 'NONE', *, *, #12573, .T. ) ;
#13441 = CARTESIAN_POINT ( 'NONE',  ( 33.25875691633515174, -58.62940108252875149, 2.501915095544871459 ) ) ;
#13442 = ADVANCED_BREP_SHAPE_REPRESENTATION ( '', ( #4356, #6315 ), #4594 ) ;
#13443 = DIRECTION ( 'NONE',  ( 1.000000000000000000, 0.000000000000000000, 0.000000000000000000 ) ) ;
#13444 = CARTESIAN_POINT ( 'NONE',  ( 48.00000000000000711, 10.25070940071368497, 33.00000000000012790 ) ) ;
#13445 = ORIENTED_EDGE ( 'NONE', *, *, #12360, .F. ) ;
#13446 = CARTESIAN_POINT ( 'NONE',  ( 29.73572575534737794, -63.50313342086874968, -3.632148419035127418 ) ) ;
#13447 = AXIS2_PLACEMENT_3D ( 'NONE', #7968, #1948, #9274 ) ;
#13448 = ORIENTED_EDGE ( 'NONE', *, *, #13590, .F. ) ;
#13449 = EDGE_CURVE ( 'NONE', #1506, #4084, #4429, .T. ) ;
#13450 = CARTESIAN_POINT ( 'NONE',  ( 29.35555050496136431, -52.24929059928631148, 3.199931146564417350 ) ) ;
#13451 = CARTESIAN_POINT ( 'NONE',  ( 96.29968967959054282, 23.25070940071369208, -33.00000000000012790 ) ) ;
#13452 = CARTESIAN_POINT ( 'NONE',  ( 52.72354942432796321, 0.2729788054883383608, 62.84860122826521689 ) ) ;
#13453 = CARTESIAN_POINT ( 'NONE',  ( 80.00000000000001421, -76.24929059928631148, 4.000000000000000000 ) ) ;
#13454 = VECTOR ( 'NONE', #5060, 1000.000000000000000 ) ;
#13455 = VERTEX_POINT ( 'NONE', #6659 ) ;
#13456 = DIRECTION ( 'NONE',  ( 0.000000000000000000, 0.000000000000000000, 1.000000000000000000 ) ) ;
#13457 = ORIENTED_EDGE ( 'NONE', *, *, #11378, .F. ) ;
#13458 = AXIS2_PLACEMENT_3D ( 'NONE', #8344, #13033, #2411 ) ;
#13459 = AXIS2_PLACEMENT_3D ( 'NONE', #9014, #4475, #6705 ) ;
#13460 = EDGE_LOOP ( 'NONE', ( #3683, #14853, #13457, #13967 ) ) ;
#13461 = ADVANCED_FACE ( 'NONE', ( #3125 ), #5732, .F. ) ;
#13462 = FACE_OUTER_BOUND ( 'NONE', #3088, .T. ) ;
#13463 = ADVANCED_FACE ( 'NONE', ( #730 ), #11076, .T. ) ;
#13464 = CONTEXT_DEPENDENT_SHAPE_REPRESENTATION ( #9092, #14917 ) ;
#13465 = DIRECTION ( 'NONE',  ( 0.8746197071345569451, -0.4848096202550666312, 0.000000000000000000 ) ) ;
#13466 = CARTESIAN_POINT ( 'NONE',  ( -5.040221427466109461, 4.089237592873833371, 58.00000000000012079 ) ) ;
#13467 = AXIS2_PLACEMENT_3D ( 'NONE', #14608, #4059, #8757 ) ;
#13468 = B_SPLINE_CURVE_WITH_KNOTS ( 'NONE', 3,
 ( #1229, #3616, #2466, #9631, #5866, #4848, #7155, #8164, #12867, #2313, #3543, #9556 ),
 .UNSPECIFIED., .F., .F.,
 ( 4, 2, 2, 2, 2, 4 ),
 ( 0.000000000000000000, 0.0002273805472697279430, 0.0004547610945394558860, 0.0009095221890789461413, 0.001364283283618436234, 0.001819044378157926543 ),
 .UNSPECIFIED. ) ;
#13469 = CARTESIAN_POINT ( 'NONE',  ( 8.766382814749736241, -57.08357682498793650, -2.747855728347990745 ) ) ;
#13470 = VERTEX_POINT ( 'NONE', #3283 ) ;
#13471 = AXIS2_PLACEMENT_3D ( 'NONE', #686, #8850, #11958 ) ;
#13472 = DIRECTION ( 'NONE',  ( -2.102695122396130409E-16, 0.000000000000000000, -1.000000000000000000 ) ) ;
#13473 = CARTESIAN_POINT ( 'NONE',  ( 65.33616866150605063, -11.06260342404821628, 71.24779283330499879 ) ) ;
#13474 = CARTESIAN_POINT ( 'NONE',  ( 62.00000000000001421, -2.249290599286310588, 38.00000000000012079 ) ) ;
#13475 = CARTESIAN_POINT ( 'NONE',  ( 17.61519226005271577, -69.39711819508849544, 6.201611931792121446 ) ) ;
#13476 = CARTESIAN_POINT ( 'NONE',  ( 13.78187932340991040, -67.90279320104012584, -3.641642753162454671 ) ) ;
#13477 = ORIENTED_EDGE ( 'NONE', *, *, #1694, .T. ) ;
#13478 = CARTESIAN_POINT ( 'NONE',  ( 56.97758043373130477, 2.707118148285912795, 48.51982618741349285 ) ) ;
#13479 = CARTESIAN_POINT ( 'NONE',  ( 20.86173033120691045, -69.39711819508849544, 0.000000000000000000 ) ) ;
#13480 = ORIENTED_EDGE ( 'NONE', *, *, #9136, .T. ) ;
#13481 = DIRECTION ( 'NONE',  ( 0.000000000000000000, 0.000000000000000000, 1.000000000000000000 ) ) ;
#13482 = LINE ( 'NONE', #7641, #6333 ) ;
#13483 = ORIENTED_EDGE ( 'NONE', *, *, #4166, .T. ) ;
#13484 = DIRECTION ( 'NONE',  ( -0.000000000000000000, 0.000000000000000000, 1.000000000000000000 ) ) ;
#13485 = EDGE_CURVE ( 'NONE', #9032, #4272, #810, .T. ) ;
#13486 = EDGE_CURVE ( 'NONE', #8564, #996, #9378, .T. ) ;
#13487 = DIRECTION ( 'NONE',  ( 1.000000000000000000, 0.000000000000000000, 0.000000000000000000 ) ) ;
#13488 = DIRECTION ( 'NONE',  ( 0.000000000000000000, -1.000000000000000000, 0.000000000000000000 ) ) ;
#13489 = AXIS2_PLACEMENT_3D ( 'NONE', #2711, #6474, #334 ) ;
#13490 = AXIS2_PLACEMENT_3D ( 'NONE', #5964, #8108, #13794 ) ;
#13491 = CARTESIAN_POINT ( 'NONE',  ( -5.290523468902621929, 4.522075770548486418, -57.50000000000012079 ) ) ;
#13492 = ORIENTED_EDGE ( 'NONE', *, *, #12153, .T. ) ;
#13493 = DIRECTION ( 'NONE',  ( 0.000000000000000000, 1.000000000000000000, -0.000000000000000000 ) ) ;
#13494 = ORIENTED_EDGE ( 'NONE', *, *, #15155, .T. ) ;
#13495 = DIRECTION ( 'NONE',  ( -0.5394184268574488961, 0.8420378618367674317, 0.000000000000000000 ) ) ;
#13496 = DIRECTION ( 'NONE',  ( -0.000000000000000000, 0.000000000000000000, 1.000000000000000000 ) ) ;
#13497 = ORIENTED_EDGE ( 'NONE', *, *, #9993, .T. ) ;
#13498 = EDGE_LOOP ( 'NONE', ( #14820, #12068, #13375, #9786 ) ) ;
#13499 = CARTESIAN_POINT ( 'NONE',  ( 100.0000000000000284, 6.750709400713692965, 139.1143251403882459 ) ) ;
#13500 = DIRECTION ( 'NONE',  ( 1.000000000000000000, 0.000000000000000000, 0.000000000000000000 ) ) ;
#13501 = VERTEX_POINT ( 'NONE', #14893 ) ;
#13502 = AXIS2_PLACEMENT_3D ( 'NONE', #6673, #13837, #12530 ) ;
#13503 = VECTOR ( 'NONE', #13698, 1000.000000000000000 ) ;
#13504 = EDGE_CURVE ( 'NONE', #14689, #6655, #658, .T. ) ;
#13505 = LINE ( 'NONE', #14882, #5953 ) ;
#13506 = EDGE_CURVE ( 'NONE', #7221, #7147, #1737, .T. ) ;
#13507 = CARTESIAN_POINT ( 'NONE',  ( 9.505449653674235222, -53.34475964609201526, 2.389227176380498641 ) ) ;
#13508 = DIRECTION ( 'NONE',  ( 0.000000000000000000, 0.000000000000000000, 1.000000000000000000 ) ) ;
#13509 = DIRECTION ( 'NONE',  ( 0.000000000000000000, 0.000000000000000000, -1.000000000000000000 ) ) ;
#13510 = AXIS2_PLACEMENT_3D ( 'NONE', #9736, #3864, #7413 ) ;
#13511 = EDGE_LOOP ( 'NONE', ( #852, #8848, #3000, #11042 ) ) ;
#13512 = CARTESIAN_POINT ( 'NONE',  ( 9.399792925529615317, -59.70501925844563118, 2.784164790581823645 ) ) ;
#13513 = VERTEX_POINT ( 'NONE', #12760 ) ;
#13514 = VERTEX_POINT ( 'NONE', #963 ) ;
#13515 = CARTESIAN_POINT ( 'NONE',  ( -16.99999999999998579, -2.249290599286303927, 38.00000000000012079 ) ) ;
#13516 = ORIENTED_EDGE ( 'NONE', *, *, #13558, .F. ) ;
#13517 = DIRECTION ( 'NONE',  ( 0.000000000000000000, 0.000000000000000000, 1.000000000000000000 ) ) ;
#13518 = CARTESIAN_POINT ( 'NONE',  ( 69.32502915396517551, -4.037540509912919795, 71.21138934095161233 ) ) ;
#13519 = EDGE_LOOP ( 'NONE', ( #13170, #6417, #3024, #9028 ) ) ;
#13520 = EDGE_CURVE ( 'NONE', #8978, #7521, #15063, .T. ) ;
#13521 = DIRECTION ( 'NONE',  ( 1.224646799147353207E-16, 1.000000000000000000, -0.000000000000000000 ) ) ;
#13522 = DIRECTION ( 'NONE',  ( 0.000000000000000000, 1.000000000000000000, 0.000000000000000000 ) ) ;
#13523 = ORIENTED_EDGE ( 'NONE', *, *, #13408, .F. ) ;
#13524 = FACE_OUTER_BOUND ( 'NONE', #9184, .T. ) ;
#13525 = VERTEX_POINT ( 'NONE', #11421 ) ;
#13526 = FACE_OUTER_BOUND ( 'NONE', #11970, .T. ) ;
#13527 = DIRECTION ( 'NONE',  ( -1.000000000000000000, 0.000000000000000000, 0.000000000000000000 ) ) ;
#13528 = CYLINDRICAL_SURFACE ( 'NONE', #1314, 1.000000000000000888 ) ;
#13529 = ORIENTED_EDGE ( 'NONE', *, *, #3189, .T. ) ;
#13530 = AXIS2_PLACEMENT_3D ( 'NONE', #12827, #6652, #877 ) ;
#13531 = DIRECTION ( 'NONE',  ( -0.000000000000000000, -0.000000000000000000, 1.000000000000000000 ) ) ;
#13532 = EDGE_LOOP ( 'NONE', ( #14054, #7539 ) ) ;
#13533 = ORIENTED_EDGE ( 'NONE', *, *, #3344, .T. ) ;
#13534 = VERTEX_POINT ( 'NONE', #4511 ) ;
#13535 = FACE_OUTER_BOUND ( 'NONE', #8687, .T. ) ;
#13536 = EDGE_CURVE ( 'NONE', #9144, #8129, #5837, .T. ) ;
#13537 = CARTESIAN_POINT ( 'NONE',  ( 0.5043391135745837195, 0.8906624217387615339, 48.00000000000012079 ) ) ;
#13538 = DIRECTION ( 'NONE',  ( 0.000000000000000000, 0.000000000000000000, 1.000000000000000000 ) ) ;
#13539 = SHAPE_REPRESENTATION ( 'Upper Sharpening Angle Guide Base', ( #6315 ), #417 ) ;
#13540 = AXIS2_PLACEMENT_3D ( 'NONE', #3493, #3332, #11644 ) ;
#13541 = LINE ( 'NONE', #4149, #10470 ) ;
#13542 = AXIS2_PLACEMENT_3D ( 'NONE', #1543, #7235, #8545 ) ;
#13543 = VERTEX_POINT ( 'NONE', #9215 ) ;
#13544 = FACE_OUTER_BOUND ( 'NONE', #8327, .T. ) ;
#13545 = EDGE_CURVE ( 'NONE', #3720, #1828, #9689, .T. ) ;
#13546 = DIRECTION ( 'NONE',  ( -1.000000000000000000, 0.000000000000000000, 0.000000000000000000 ) ) ;
#13547 = DIRECTION ( 'NONE',  ( 1.000000000000000000, 8.673617379884035472E-17, 0.000000000000000000 ) ) ;
#13548 = EDGE_CURVE ( 'NONE', #5507, #8849, #1048, .T. ) ;
#13549 = ORIENTED_EDGE ( 'NONE', *, *, #6325, .T. ) ;
#13550 = AXIS2_PLACEMENT_3D ( 'NONE', #6401, #12176, #7415 ) ;
#13551 = CARTESIAN_POINT ( 'NONE',  ( 33.59512494182110487, -55.93948076112101120, 2.601440957439760115 ) ) ;
#13552 = AXIS2_PLACEMENT_3D ( 'NONE', #1304, #10775, #10698 ) ;
#13553 = CIRCLE ( 'NONE', #12584, 11.46463184759105403 ) ;
#13554 = LINE ( 'NONE', #14490, #6869 ) ;
#13555 = ORIENTED_EDGE ( 'NONE', *, *, #15142, .T. ) ;
#13556 = LINE ( 'NONE', #2086, #8639 ) ;
#13557 = DIRECTION ( 'NONE',  ( 0.000000000000000000, 0.000000000000000000, 1.000000000000000000 ) ) ;
#13558 = EDGE_CURVE ( 'NONE', #7966, #6896, #5991, .T. ) ;
#13559 = DIRECTION ( 'NONE',  ( 0.8746197071345569451, -0.4848096202550666312, 0.000000000000000000 ) ) ;
#13560 = EDGE_LOOP ( 'NONE', ( #14562, #11843, #4818, #8297 ) ) ;
#13561 = CARTESIAN_POINT ( 'NONE',  ( -1.197457146693716057, -2.220571218158943427, 48.00000000000012079 ) ) ;
#13562 = AXIS2_PLACEMENT_3D ( 'NONE', #10944, #464, #2557 ) ;
#13563 = VECTOR ( 'NONE', #13729, 1000.000000000000000 ) ;
#13564 = AXIS2_PLACEMENT_3D ( 'NONE', #11469, #5727, #2246 ) ;
#13565 = FACE_OUTER_BOUND ( 'NONE', #479, .T. ) ;
#13566 = DIRECTION ( 'NONE',  ( -1.000000000000000000, 0.000000000000000000, 0.000000000000000000 ) ) ;
#13567 = DIRECTION ( 'NONE',  ( 2.775557561562891351E-15, -1.000000000000000000, 0.000000000000000000 ) ) ;
#13568 = ORIENTED_EDGE ( 'NONE', *, *, #3153, .T. ) ;
#13569 = DIRECTION ( 'NONE',  ( -1.000000000000000000, 0.000000000000000000, 0.000000000000000000 ) ) ;
#13570 = EDGE_CURVE ( 'NONE', #3333, #4512, #5182, .T. ) ;
#13571 = ORIENTED_EDGE ( 'NONE', *, *, #13638, .T. ) ;
#13572 = CARTESIAN_POINT ( 'NONE',  ( 23.47858629692700561, -53.24929059928630437, -6.492462156583982846 ) ) ;
#13573 = DIRECTION ( 'NONE',  ( -1.000000000000000000, -1.156482317317870492E-16, 0.000000000000000000 ) ) ;
#13574 = AXIS2_PLACEMENT_3D ( 'NONE', #15088, #15003, #984 ) ;
#13575 = ORIENTED_EDGE ( 'NONE', *, *, #3828, .T. ) ;
#13577 = VERTEX_POINT ( 'NONE', #12915 ) ;
#13576 = LINE ( 'NONE', #4179, #6458 ) ;
#13578 = CARTESIAN_POINT ( 'NONE',  ( 0.000000000000000000, 0.000000000000000000, 58.00000000000012079 ) ) ;
#13579 = AXIS2_PLACEMENT_3D ( 'NONE', #2668, #7364, #12052 ) ;
#13580 = CARTESIAN_POINT ( 'NONE',  ( 12.41997800841365773, -64.16417350152165966, 3.791131921655388037 ) ) ;
#13581 = CARTESIAN_POINT ( 'NONE',  ( 56.97758043373130477, 2.707118148285912795, 62.84860122826521689 ) ) ;
#13582 = CARTESIAN_POINT ( 'NONE',  ( 33.48164203564194707, -55.39134602458726420, -1.947764125980440797 ) ) ;
#13583 = PRODUCT ( 'Small Aluminum Top-Plate Insert', 'Small Aluminum Top-Plate Insert', '', ( #12164 ) ) ;
#13584 = AXIS2_PLACEMENT_3D ( 'NONE', #1211, #4827, #5922 ) ;
#13585 = DIRECTION ( 'NONE',  ( -0.000000000000000000, -0.000000000000000000, 1.000000000000000000 ) ) ;
#13586 = CYLINDRICAL_SURFACE ( 'NONE', #199, 4.000000000000003553 ) ;
#13587 = AXIS2_PLACEMENT_3D ( 'NONE', #10938, #9716, #6170 ) ;
#13588 = EDGE_LOOP ( 'NONE', ( #14919, #12732 ) ) ;
#13589 = ADVANCED_FACE ( 'NONE', ( #14285 ), #10350, .F. ) ;
#13590 = EDGE_CURVE ( 'NONE', #12406, #10773, #10852, .T. ) ;
#13591 = VERTEX_POINT ( 'NONE', #11897 ) ;
#13592 = CARTESIAN_POINT ( 'NONE',  ( 8.091875466796993877, -56.84741961274605160, 1.823451407584537609 ) ) ;
#13593 = ORIENTED_EDGE ( 'NONE', *, *, #8646, .T. ) ;
#13594 = DIRECTION ( 'NONE',  ( -0.000000000000000000, -0.000000000000000000, -1.000000000000000000 ) ) ;
#13595 = CARTESIAN_POINT ( 'NONE',  ( 69.46454297106447484, -2.294433322023681221, 73.06560708801610815 ) ) ;
#13596 = B_SPLINE_CURVE_WITH_KNOTS ( 'NONE', 3,
 ( #7137, #8139, #6986, #9452, #8062, #3363 ),
 .UNSPECIFIED., .F., .F.,
 ( 4, 2, 4 ),
 ( 0.001000432843099107122, 0.009082381923694659437, 0.01716433100429023278 ),
 .UNSPECIFIED. ) ;
#13597 = B_SPLINE_CURVE_WITH_KNOTS ( 'NONE', 3,
 ( #13425, #13896, #7126, #2431, #8213, #9441, #12907, #1200 ),
 .UNSPECIFIED., .F., .F.,
 ( 4, 2, 2, 4 ),
 ( 0.000000000000000000, 0.0002685268308981082351, 0.0005370536617962164702, 0.001074107323592430338 ),
 .UNSPECIFIED. ) ;
#13598 = VECTOR ( 'NONE', #3349, 1000.000000000000000 ) ;
#13599 = DIRECTION ( 'NONE',  ( 0.8208219420614805140, -0.4549890321264307702, -0.3453061251629823691 ) ) ;
#13600 = DIRECTION ( 'NONE',  ( -0.000000000000000000, 1.000000000000000000, -0.000000000000000000 ) ) ;
#13601 = ORIENTED_EDGE ( 'NONE', *, *, #8397, .T. ) ;
#13602 = AXIS2_PLACEMENT_3D ( 'NONE', #10535, #4368, #11518 ) ;
#13603 = CARTESIAN_POINT ( 'NONE',  ( -16.99999999999998579, -2.249290599286303927, -38.00000000000012079 ) ) ;
#13604 = ORIENTED_EDGE ( 'NONE', *, *, #9123, .T. ) ;
#13605 = CARTESIAN_POINT ( 'NONE',  ( 67.21328690825531282, 22.43695620243006772, 33.00000000000012790 ) ) ;
#13606 = CARTESIAN_POINT ( 'NONE',  ( -8.499999999999987566, -2.249290599286303927, 38.50000000000012790 ) ) ;
#13607 = CARTESIAN_POINT ( 'NONE',  ( -16.99999999999998579, -2.249290599286303927, -47.50000000000012079 ) ) ;
#13608 = DIRECTION ( 'NONE',  ( -0.8656763553493062036, -0.5006040828730242698, 0.000000000000000000 ) ) ;
#13609 = EDGE_LOOP ( 'NONE', ( #13059, #11387, #11098 ) ) ;
#13610 = EDGE_CURVE ( 'NONE', #6567, #3269, #5830, .T. ) ;
#13611 = EDGE_CURVE ( 'NONE', #13470, #1907, #8144, .T. ) ;
#13612 = LINE ( 'NONE', #12305, #4877 ) ;
#13613 = VERTEX_POINT ( 'NONE', #2358 ) ;
#13614 = ORIENTED_EDGE ( 'NONE', *, *, #8194, .F. ) ;
#13615 = ORIENTED_EDGE ( 'NONE', *, *, #476, .F. ) ;
#13616 = DIRECTION ( 'NONE',  ( -0.8420378618367651002, -0.5394184268574528929, -2.807225425332302624E-15 ) ) ;
#13617 = CARTESIAN_POINT ( 'NONE',  ( 8.700745695602643437, -59.65359113318982054, -1.835578343538661672 ) ) ;
#13618 = CARTESIAN_POINT ( 'NONE',  ( -22.95637227168126770, 4.533106128208347130, -48.03392779025640635 ) ) ;
#13619 = DIRECTION ( 'NONE',  ( 1.000000000000000000, 0.000000000000000000, 0.000000000000000000 ) ) ;
#13620 = ORIENTED_EDGE ( 'NONE', *, *, #707, .T. ) ;
#13621 = CARTESIAN_POINT ( 'NONE',  ( 66.24588231955848983, -11.54213538233861236, 72.19766410831374515 ) ) ;
#13622 = CARTESIAN_POINT ( 'NONE',  ( 32.98169228882561299, -56.83327624868833539, -2.758240060640952951 ) ) ;
#13623 = CARTESIAN_POINT ( 'NONE',  ( -9.358536206588548012, 2.506280377409947135, 47.89606589046130125 ) ) ;
#13624 = CARTESIAN_POINT ( 'NONE',  ( 12.66974950169169567, -64.60713873539394569, -3.212402267258147592 ) ) ;
#13625 = VERTEX_POINT ( 'NONE', #7049 ) ;
#13626 = CARTESIAN_POINT ( 'NONE',  ( -0.9277479332649583021, -2.641590149077306826, 57.50000000000012079 ) ) ;
#13627 = CARTESIAN_POINT ( 'NONE',  ( -5.040221427466046400, 4.089237592873870675, -48.00000000000012079 ) ) ;
#13628 = ADVANCED_FACE ( 'NONE', ( #2284 ), #2735, .T. ) ;
#13629 = ORIENTED_EDGE ( 'NONE', *, *, #9277, .F. ) ;
#13630 = SURFACE_SIDE_STYLE ('',( #10097 ) ) ;
#13631 =( BOUNDED_SURFACE ( )  B_SPLINE_SURFACE ( 3, 2, ( 
 ( #11404, #4408, #2183 ),
 ( #7962, #6794, #9112 ),
 ( #9031, #11482, #8113 ),
 ( #15038, #12495, #4490 ),
 ( #1942, #6875, #13726 ),
 ( #11560, #4252, #6958 ) ),
 .UNSPECIFIED., .F., .F., .F. ) 
 B_SPLINE_SURFACE_WITH_KNOTS ( ( 4, 2, 4 ),
 ( 3, 3 ),
 ( 1.084202172485504434E-19, 0.001005789800061012871, 0.002011579600122025743 ),
 ( 0.000000000000000000, 1.000000000000000000 ),
 .UNSPECIFIED. ) 
 GEOMETRIC_REPRESENTATION_ITEM ( )  RATIONAL_B_SPLINE_SURFACE ( (
 ( 1.000000000000000000, 0.8308543624379417514, 1.000000000000000000),
 ( 1.000000000000000000, 0.8317114229144060289, 1.000000000000000000),
 ( 1.000000000000000000, 0.8301458553065871326, 1.000000000000000000),
 ( 1.000000000000000000, 0.8215594255318671157, 1.000000000000000000),
 ( 1.000000000000000000, 0.8147253674582816130, 1.000000000000000000),
 ( 1.000000000000000000, 0.8053615646146046192, 1.000000000000000000) ) ) 
 REPRESENTATION_ITEM ( '' )  SURFACE ( )  );
#13632 = LINE ( 'NONE', #11393, #9831 ) ;
#13633 = LINE ( 'NONE', #775, #13954 ) ;
#13634 = CARTESIAN_POINT ( 'NONE',  ( -16.99999999999998579, -2.249290599286303927, -50.50000000000012079 ) ) ;
#13635 = ORIENTED_EDGE ( 'NONE', *, *, #13123, .T. ) ;
#13636 = EDGE_CURVE ( 'NONE', #7134, #7276, #6057, .T. ) ;
#13637 = LINE ( 'NONE', #7494, #4334 ) ;
#13638 = EDGE_CURVE ( 'NONE', #9843, #9144, #8726, .T. ) ;
#13639 = FACE_OUTER_BOUND ( 'NONE', #6242, .T. ) ;
#13640 = DIRECTION ( 'NONE',  ( -0.000000000000000000, -0.000000000000000000, -1.000000000000000000 ) ) ;
#13641 = EDGE_CURVE ( 'NONE', #3355, #13079, #5194, .T. ) ;
#13642 = CYLINDRICAL_SURFACE ( 'NONE', #1513, 3.000000000000000888 ) ;
#13643 = EDGE_CURVE ( 'NONE', #11505, #4816, #57, .T. ) ;
#13644 = ORIENTED_EDGE ( 'NONE', *, *, #1790, .F. ) ;
#13645 = CARTESIAN_POINT ( 'NONE',  ( -16.99999999999998579, -2.249290599286303927, -47.31370849898487307 ) ) ;
#13646 = VERTEX_POINT ( 'NONE', #10522 ) ;
#13647 = LINE ( 'NONE', #944, #8404 ) ;
#13648 = CARTESIAN_POINT ( 'NONE',  ( 8.538156564172162177, -54.60220113588928115, 2.070297547960220808 ) ) ;
#13649 = EDGE_CURVE ( 'NONE', #7206, #7233, #11088, .T. ) ;
#13650 = ORIENTED_EDGE ( 'NONE', *, *, #74, .T. ) ;
#13652 = VERTEX_POINT ( 'NONE', #6979 ) ;
#13651 = CARTESIAN_POINT ( 'NONE',  ( 40.00000000000001421, -74.24929059928631148, -33.00000000000000000 ) ) ;
#13653 = PLANE ( 'NONE',  #12445 ) ;
#13654 = EDGE_CURVE ( 'NONE', #1474, #788, #9289, .T. ) ;
#13655 = ADVANCED_FACE ( 'NONE', ( #5911 ), #9447, .T. ) ;
#13656 = CARTESIAN_POINT ( 'NONE',  ( 8.890669559332980754, -60.05631636466448953, -1.868376189747823046 ) ) ;
#13657 = CIRCLE ( 'NONE', #397, 0.5000000000000003331 ) ;
#13658 = CARTESIAN_POINT ( 'NONE',  ( 11.13121913594275370, -52.42016302384273985, 2.859972208322074660 ) ) ;
#13659 = CARTESIAN_POINT ( 'NONE',  ( 33.26342499051592938, -54.78204083127141644, -2.039726671434834770 ) ) ;
#13660 = DIRECTION ( 'NONE',  ( -1.000000000000000000, 0.000000000000000000, 0.000000000000000000 ) ) ;
#13661 = CARTESIAN_POINT ( 'NONE',  ( 25.18496984658901638, -69.39711819508849544, 5.637959728397568426 ) ) ;
#13662 = CARTESIAN_POINT ( 'NONE',  ( 58.92629142760364402, 23.25070940071368852, 33.00000000000012790 ) ) ;
#13663 = ORIENTED_EDGE ( 'NONE', *, *, #14907, .T. ) ;
#13664 = CARTESIAN_POINT ( 'NONE',  ( 9.273438744392825228, -59.39772283578258794, 2.758706911751842128 ) ) ;
#13665 = ORIENTED_EDGE ( 'NONE', *, *, #2430, .T. ) ;
#13666 = DIRECTION ( 'NONE',  ( 0.000000000000000000, 0.000000000000000000, -1.000000000000000000 ) ) ;
#13667 = ORIENTED_EDGE ( 'NONE', *, *, #14162, .T. ) ;
#13668 = DIRECTION ( 'NONE',  ( 1.000000000000000000, 0.000000000000000000, -0.000000000000000000 ) ) ;
#13669 = VECTOR ( 'NONE', #5292, 1000.000000000000000 ) ;
#13670 = DIRECTION ( 'NONE',  ( 0.000000000000000000, 0.000000000000000000, -1.000000000000000000 ) ) ;
#13671 = LINE ( 'NONE', #1966, #5581 ) ;
#13672 = LINE ( 'NONE', #11508, #11386 ) ;
#13673 = EDGE_LOOP ( 'NONE', ( #894, #631, #5531, #2319 ) ) ;
#13674 = DIRECTION ( 'NONE',  ( 1.000000000000000000, 0.000000000000000000, 0.000000000000000000 ) ) ;
#13675 = ORIENTED_EDGE ( 'NONE', *, *, #8381, .F. ) ;
#13676 = EDGE_CURVE ( 'NONE', #9571, #4786, #1275, .T. ) ;
#13677 = VECTOR ( 'NONE', #592, 1000.000000000000000 ) ;
#13678 = VECTOR ( 'NONE', #9219, 1000.000000000000000 ) ;
#13679 = LINE ( 'NONE', #5532, #7607 ) ;
#13680 = CARTESIAN_POINT ( 'NONE',  ( 8.090375438032983979, -56.83262086368637256, -1.823905708655537028 ) ) ;
#13681 = CARTESIAN_POINT ( 'NONE',  ( -16.99999999999998579, -2.249290599286303927, -57.50000000000012079 ) ) ;
#13682 = CARTESIAN_POINT ( 'NONE',  ( 54.85055839958032209, 23.25070940071368852, 139.1143251403882459 ) ) ;
#13683 = ORIENTED_EDGE ( 'NONE', *, *, #3414, .T. ) ;
#13684 = VERTEX_POINT ( 'NONE', #13058 ) ;
#13685 = CYLINDRICAL_SURFACE ( 'NONE', #928, 6.484807146443463566 ) ;
#13686 = VECTOR ( 'NONE', #14135, 1000.000000000000000 ) ;
#13687 = VERTEX_POINT ( 'NONE', #12268 ) ;
#13688 = CARTESIAN_POINT ( 'NONE',  ( -2.688903428702175252E-15, 23.25070940071368142, -33.00000000000012790 ) ) ;
#13689 = AXIS2_PLACEMENT_3D ( 'NONE', #4863, #8098, #8181 ) ;
#13690 = EDGE_LOOP ( 'NONE', ( #4386, #13022, #12576, #12151 ) ) ;
#13691 = ORIENTED_EDGE ( 'NONE', *, *, #7824, .F. ) ;
#13693 = VECTOR ( 'NONE', #5077, 1000.000000000000000 ) ;
#13692 = CARTESIAN_POINT ( 'NONE',  ( -65.00000000000001421, -85.24929059928629727, -17.50000000000000000 ) ) ;
#13694 = CIRCLE ( 'NONE', #8042, 4.194885682587998765 ) ;
#13695 = CARTESIAN_POINT ( 'NONE',  ( 9.272883950264748876, -59.39518542680082192, -2.758694842813115056 ) ) ;
#13696 = CARTESIAN_POINT ( 'NONE',  ( -24.72817752516938228, 2.363221963240404566, -47.50000000000012079 ) ) ;
#13697 = EDGE_CURVE ( 'NONE', #10500, #6582, #5271, .T. ) ;
#13698 = DIRECTION ( 'NONE',  ( -0.000000000000000000, -0.000000000000000000, -1.000000000000000000 ) ) ;
#13699 = DIRECTION ( 'NONE',  ( 0.8746197071345570562, -0.4848096202550665756, 0.000000000000000000 ) ) ;
#13700 = EDGE_CURVE ( 'NONE', #4038, #1083, #9750, .T. ) ;
#13701 = ORIENTED_EDGE ( 'NONE', *, *, #4799, .F. ) ;
#13702 = VECTOR ( 'NONE', #3514, 1000.000000000000000 ) ;
#13703 = EDGE_LOOP ( 'NONE', ( #12540, #13593, #10381, #14944 ) ) ;
#13704 = DIRECTION ( 'NONE',  ( -0.000000000000000000, 1.000000000000000000, 1.445602896647339163E-16 ) ) ;
#13705 = LINE ( 'NONE', #7269, #3406 ) ;
#13706 = CARTESIAN_POINT ( 'NONE',  ( 69.44125642334664406, -2.986918215369366081, 76.69762336658895663 ) ) ;
#13707 = VECTOR ( 'NONE', #15164, 1000.000000000000000 ) ;
#13708 = CARTESIAN_POINT ( 'NONE',  ( 57.83740799265796539, -7.800393779465814248, 54.56811043785582882 ) ) ;
#13709 = CARTESIAN_POINT ( 'NONE',  ( 24.18480965113672099, -70.79589105105083036, 6.161139702147667485 ) ) ;
#13710 = ORIENTED_EDGE ( 'NONE', *, *, #10653, .F. ) ;
#13711 = AXIS2_PLACEMENT_3D ( 'NONE', #11313, #2008, #11468 ) ;
#13712 = CARTESIAN_POINT ( 'NONE',  ( 69.46051462023766021, -2.575682430178798832, 72.15988747666172287 ) ) ;
#13713 = CARTESIAN_POINT ( 'NONE',  ( -8.537170960192302260, 2.067018546614597163, 48.00000000000012079 ) ) ;
#13714 = VERTEX_POINT ( 'NONE', #14368 ) ;
#13715 = CARTESIAN_POINT ( 'NONE',  ( -2.688903428702175252E-15, 23.25070940071368142, 139.1143251403882459 ) ) ;
#13716 = DIRECTION ( 'NONE',  ( 0.8746197071345569451, -0.4848096202550666312, 0.000000000000000000 ) ) ;
#13717 = EDGE_LOOP ( 'NONE', ( #7375, #11118, #7062, #9255, #7317, #8960 ) ) ;
#13718 = VECTOR ( 'NONE', #13792, 1000.000000000000000 ) ;
#13719 = FACE_BOUND ( 'NONE', #9424, .T. ) ;
#13720 = DIRECTION ( 'NONE',  ( 1.000000000000000000, 0.000000000000000000, 0.000000000000000000 ) ) ;
#13721 = DIRECTION ( 'NONE',  ( -0.000000000000000000, -1.000000000000000000, -0.000000000000000000 ) ) ;
#13722 = CARTESIAN_POINT ( 'NONE',  ( -25.99999999999998934, -2.249290599286303927, 58.00000000000012079 ) ) ;
#13723 = FACE_OUTER_BOUND ( 'NONE', #2117, .T. ) ;
#13724 = ORIENTED_EDGE ( 'NONE', *, *, #5564, .F. ) ;
#13725 = EDGE_LOOP ( 'NONE', ( #12787, #636, #4412, #4919 ) ) ;
#13726 = CARTESIAN_POINT ( 'NONE',  ( 32.06857839880813543, -61.15288932781299991, 2.038807541295255543 ) ) ;
#13727 = ORIENTED_EDGE ( 'NONE', *, *, #9981, .F. ) ;
#13728 = CARTESIAN_POINT ( 'NONE',  ( 25.54537353427514645, -52.24929059928631148, -5.670202843350166333 ) ) ;
#13729 = DIRECTION ( 'NONE',  ( 0.000000000000000000, -1.000000000000000000, 0.000000000000000000 ) ) ;
#13730 = EDGE_CURVE ( 'NONE', #11720, #8531, #8720, .T. ) ;
#13731 = ORIENTED_EDGE ( 'NONE', *, *, #9727, .F. ) ;
#13732 = DIRECTION ( 'NONE',  ( -0.000000000000000000, 0.000000000000000000, -1.000000000000000000 ) ) ;
#13733 = CYLINDRICAL_SURFACE ( 'NONE', #1395, 0.4999999999999996114 ) ;
#13734 = EDGE_CURVE ( 'NONE', #13354, #7451, #571, .T. ) ;
#13735 = CARTESIAN_POINT ( 'NONE',  ( 13.12221348233057050, -65.57050171853551035, 4.044987206838578153 ) ) ;
#13736 = CARTESIAN_POINT ( 'NONE',  ( -80.00000000000001421, -74.24929059928631148, -8.000000000000001776 ) ) ;
#13737 = DIRECTION ( 'NONE',  ( 0.4848096202550658540, 0.8746197071345573892, 0.000000000000000000 ) ) ;
#13738 = DIRECTION ( 'NONE',  ( 0.000000000000000000, 1.000000000000000000, -0.000000000000000000 ) ) ;
#13739 = CARTESIAN_POINT ( 'NONE',  ( 32.39917484285220439, 0.000000000000000000, 33.00000000000012790 ) ) ;
#13740 = DIRECTION ( 'NONE',  ( 0.000000000000000000, -1.000000000000000000, -1.734723475976805517E-15 ) ) ;
#13741 = EDGE_CURVE ( 'NONE', #7624, #12008, #12033, .T. ) ;
#13742 = VERTEX_POINT ( 'NONE', #5191 ) ;
#13743 = EDGE_CURVE ( 'NONE', #1788, #1844, #8653, .T. ) ;
#13744 = CARTESIAN_POINT ( 'NONE',  ( 18.22133905414316501, -54.09900330348973085, -6.482993899727721221 ) ) ;
#13745 = ORIENTED_EDGE ( 'NONE', *, *, #1604, .T. ) ;
#13746 = VECTOR ( 'NONE', #10319, 1000.000000000000114 ) ;
#13747 = CARTESIAN_POINT ( 'NONE',  ( 32.64893527110322680, -58.48797006926987052, -2.754379914540423968 ) ) ;
#13748 = CIRCLE ( 'NONE', #7121, 0.7892041907098322762 ) ;
#13749 = VERTEX_POINT ( 'NONE', #3886 ) ;
#13750 = DIRECTION ( 'NONE',  ( 0.8746197071345560570, -0.4848096202550682410, 0.000000000000000000 ) ) ;
#13751 = CARTESIAN_POINT ( 'NONE',  ( 95.31453344691183815, 21.75070940071356418, 139.1143251403882459 ) ) ;
#13752 = CARTESIAN_POINT ( 'NONE',  ( 98.40734512546775647, 21.75070940071359615, 33.00000000000012790 ) ) ;
#13753 = CARTESIAN_POINT ( 'NONE',  ( -16.99999999999998579, -2.249290599286303927, 38.00000000000012079 ) ) ;
#13754 = DIRECTION ( 'NONE',  ( 0.000000000000000000, 1.000000000000000000, 0.000000000000000000 ) ) ;
#13755 = EDGE_LOOP ( 'NONE', ( #2730, #13999, #8987, #9853 ) ) ;
#13756 = VECTOR ( 'NONE', #7334, 1000.000000000000000 ) ;
#13757 = CARTESIAN_POINT ( 'NONE',  ( 66.11049071757111051, -11.60217708172952022, 76.17393377513106145 ) ) ;
#13758 = CARTESIAN_POINT ( 'NONE',  ( 9.782925212513372770, -53.09518070810211299, -3.364836540200758286 ) ) ;
#13759 = CARTESIAN_POINT ( 'NONE',  ( 68.02719294894561131, -7.807454411681060691, 82.40005259842790508 ) ) ;
#13760 = CARTESIAN_POINT ( 'NONE',  ( 59.12196317473677709, -7.688259372168277928, 60.61639468829817190 ) ) ;
#13761 = ORIENTED_EDGE ( 'NONE', *, *, #4537, .F. ) ;
#13762 = CARTESIAN_POINT ( 'NONE',  ( -16.99999999999998579, -2.249290599286303927, -58.00000000000012079 ) ) ;
#13763 = VERTEX_POINT ( 'NONE', #6215 ) ;
#13764 = CARTESIAN_POINT ( 'NONE',  ( -30.00000000000000000, -72.24929059928631148, -32.99999999999999289 ) ) ;
#13765 = EDGE_LOOP ( 'NONE', ( #3519, #11995, #3703, #1132, #14975, #7693, #3906, #6510, #14063, #8855, #11357, #4585, #365 ) ) ;
#13766 = VERTEX_POINT ( 'NONE', #14579 ) ;
#13767 = EDGE_CURVE ( 'NONE', #7109, #12771, #14295, .T. ) ;
#13768 = AXIS2_PLACEMENT_3D ( 'NONE', #12838, #11423, #13750 ) ;
#13769 = CARTESIAN_POINT ( 'NONE',  ( 65.00000000000001421, -85.24929059928629727, -19.99999999999999645 ) ) ;
#13770 = LINE ( 'NONE', #4222, #6950 ) ;
#13771 = CARTESIAN_POINT ( 'NONE',  ( -16.99999999999998579, -2.249290599286303927, 38.50000000000012790 ) ) ;
#13772 = CARTESIAN_POINT ( 'NONE',  ( 96.00000000000002842, 6.750709400713692965, 139.1143251403882459 ) ) ;
#13773 = ORIENTED_EDGE ( 'NONE', *, *, #9616, .F. ) ;
#13774 = PLANE ( 'NONE',  #14673 ) ;
#13775 = DIRECTION ( 'NONE',  ( 0.000000000000000000, 0.000000000000000000, 1.000000000000000000 ) ) ;
#13776 = CARTESIAN_POINT ( 'NONE',  ( 29.69047892279255407, -53.28399145779480506, -4.141535524925019196 ) ) ;
#13777 = CYLINDRICAL_SURFACE ( 'NONE', #15085, 4.000000000000000000 ) ;
#13778 = CARTESIAN_POINT ( 'NONE',  ( 27.83979445996965296, -68.65220048136343678, 4.053998922580534625 ) ) ;
#13779 = ORIENTED_EDGE ( 'NONE', *, *, #5040, .F. ) ;
#13780 = CARTESIAN_POINT ( 'NONE',  ( 70.00558585377599741, -3.250648700864071206, 72.86275793890305863 ) ) ;
#13781 = CYLINDRICAL_SURFACE ( 'NONE', #2225, 4.194885682587998765 ) ;
#13782 = VECTOR ( 'NONE', #11586, 1000.000000000000000 ) ;
#13783 = ORIENTED_EDGE ( 'NONE', *, *, #11242, .T. ) ;
#13784 = EDGE_CURVE ( 'NONE', #7863, #5523, #1431, .T. ) ;
#13785 = DIRECTION ( 'NONE',  ( -0.000000000000000000, 1.000000000000000000, -0.000000000000000000 ) ) ;
#13786 = CARTESIAN_POINT ( 'NONE',  ( 33.52235686305655804, -57.48563641131178770, 2.500000000000000000 ) ) ;
#13787 = ORIENTED_EDGE ( 'NONE', *, *, #8126, .T. ) ;
#13788 = AXIS2_PLACEMENT_3D ( 'NONE', #3916, #5228, #9930 ) ;
#13789 = DIRECTION ( 'NONE',  ( 0.000000000000000000, 0.000000000000000000, 1.000000000000000000 ) ) ;
#13790 = CARTESIAN_POINT ( 'NONE',  ( 54.86190032082818391, 1.721056973166403603, 60.61639468829817190 ) ) ;
#13791 = VECTOR ( 'NONE', #8581, 1000.000000000000000 ) ;
#13792 = DIRECTION ( 'NONE',  ( -0.000000000000000000, -0.000000000000000000, 1.000000000000000000 ) ) ;
#13793 = CARTESIAN_POINT ( 'NONE',  ( 32.97418302199919538, -56.32592369292858336, 2.799485268159561890 ) ) ;
#13794 = DIRECTION ( 'NONE',  ( 1.000000000000000000, 0.000000000000000000, 0.000000000000000000 ) ) ;
#13795 = FACE_OUTER_BOUND ( 'NONE', #12557, .T. ) ;
#13796 = AXIS2_PLACEMENT_3D ( 'NONE', #9343, #2335, #14033 ) ;
#13797 = ORIENTED_EDGE ( 'NONE', *, *, #5761, .F. ) ;
#13798 = ORIENTED_EDGE ( 'NONE', *, *, #14118, .F. ) ;
#13799 = EDGE_CURVE ( 'NONE', #1184, #4603, #6136, .T. ) ;
#13800 = DIRECTION ( 'NONE',  ( 0.000000000000000000, 1.000000000000000000, 0.000000000000000000 ) ) ;
#13801 = ORIENTED_EDGE ( 'NONE', *, *, #2601, .T. ) ;
#13802 = FACE_BOUND ( 'NONE', #1689, .T. ) ;
#13803 = DIRECTION ( 'NONE',  ( -0.000000000000000000, -0.000000000000000000, -1.000000000000000000 ) ) ;
#13804 = VERTEX_POINT ( 'NONE', #2877 ) ;
#13805 = DIRECTION ( 'NONE',  ( -0.8746197071345569451, 0.4848096202550666312, 0.000000000000000000 ) ) ;
#13806 = DIRECTION ( 'NONE',  ( 0.000000000000000000, 0.000000000000000000, 1.000000000000000000 ) ) ;
#13807 = CIRCLE ( 'NONE', #11106, 0.5000000000000004441 ) ;
#13808 = DIRECTION ( 'NONE',  ( 0.8746197071345560570, -0.4848096202550682410, 0.000000000000000000 ) ) ;
#13809 = ADVANCED_FACE ( 'NONE', ( #13209 ), #7166, .T. ) ;
#13810 = DIRECTION ( 'NONE',  ( 0.000000000000000000, 0.000000000000000000, 1.000000000000000000 ) ) ;
#13811 = CARTESIAN_POINT ( 'NONE',  ( 32.87706978204689534, -54.07871170900528313, -2.179395260058141215 ) ) ;
#13812 = DIRECTION ( 'NONE',  ( 0.000000000000000000, -1.000000000000000000, -1.682156097916903736E-15 ) ) ;
#13813 = CARTESIAN_POINT ( 'NONE',  ( -80.00000000000001421, -74.24929059928631148, -4.000000000000000000 ) ) ;
#13814 = VECTOR ( 'NONE', #8959, 1000.000000000000000 ) ;
#13815 = AXIS2_PLACEMENT_3D ( 'NONE', #10115, #4256, #4494 ) ;
#13816 = CARTESIAN_POINT ( 'NONE',  ( -16.99999999999998579, -67.96969602390581144, -32.99999999999998579 ) ) ;
#13817 = CIRCLE ( 'NONE', #4975, 0.4999999999999995559 ) ;
#13818 = ORIENTED_EDGE ( 'NONE', *, *, #14946, .F. ) ;
#13819 = CARTESIAN_POINT ( 'NONE',  ( 12.57791131244190197, -50.05638191677160620, -4.212312498554237727 ) ) ;
#13820 = VECTOR ( 'NONE', #1072, 1000.000000000000000 ) ;
#13821 = ORIENTED_EDGE ( 'NONE', *, *, #13825, .F. ) ;
#13822 = DIRECTION ( 'NONE',  ( 1.000000000000000000, 0.000000000000000000, 0.000000000000000000 ) ) ;
#13823 = ORIENTED_EDGE ( 'NONE', *, *, #14279, .T. ) ;
#13824 = FILL_AREA_STYLE_COLOUR ( '', #4424 ) ;
#13825 = EDGE_CURVE ( 'NONE', #13251, #14077, #280, .T. ) ;
#13826 = DIRECTION ( 'NONE',  ( -1.000000000000000000, 0.000000000000000000, 0.000000000000000000 ) ) ;
#13827 = AXIS2_PLACEMENT_3D ( 'NONE', #6121, #1104, #14042 ) ;
#13828 = CARTESIAN_POINT ( 'NONE',  ( 70.26445833701072274, -4.474174595298148205, 76.19766410831374515 ) ) ;
#13829 = LINE ( 'NONE', #14900, #14831 ) ;
#13830 = EDGE_CURVE ( 'NONE', #8112, #7744, #10862, .T. ) ;
#13831 = EDGE_CURVE ( 'NONE', #9446, #12466, #13350, .T. ) ;
#13832 = FACE_BOUND ( 'NONE', #11301, .T. ) ;
#13833 = EDGE_CURVE ( 'NONE', #7182, #7033, #4514, .T. ) ;
#13834 = AXIS2_PLACEMENT_3D ( 'NONE', #5132, #7512, #9836 ) ;
#13835 = VERTEX_POINT ( 'NONE', #8514 ) ;
#13836 = CIRCLE ( 'NONE', #2033, 4.000000000000003553 ) ;
#13837 = DIRECTION ( 'NONE',  ( 0.000000000000000000, -0.000000000000000000, 1.000000000000000000 ) ) ;
#13838 = CARTESIAN_POINT ( 'NONE',  ( 9.122196393684426141, -53.72848551507318859, -3.102677277819655632 ) ) ;
#13839 = DIRECTION ( 'NONE',  ( 0.000000000000000000, 0.000000000000000000, -1.000000000000000000 ) ) ;
#13840 = DIRECTION ( 'NONE',  ( 0.000000000000000000, -1.000000000000000000, 0.000000000000000000 ) ) ;
#13841 = EDGE_CURVE ( 'NONE', #5929, #13543, #12126, .T. ) ;
#13842 = ORIENTED_EDGE ( 'NONE', *, *, #2217, .T. ) ;
#13843 = CARTESIAN_POINT ( 'NONE',  ( 32.52281604437752804, -59.06479067038042530, 2.757123406423269696 ) ) ;
#13844 = ORIENTED_EDGE ( 'NONE', *, *, #8530, .F. ) ;
#13845 = CARTESIAN_POINT ( 'NONE',  ( 9.175559494770812563, -57.26105658658105568, -1.816685854991390014 ) ) ;
#13846 = ORIENTED_EDGE ( 'NONE', *, *, #9195, .T. ) ;
#13847 = AXIS2_PLACEMENT_3D ( 'NONE', #1814, #5281, #2892 ) ;
#13848 = VECTOR ( 'NONE', #12449, 1000.000000000000000 ) ;
#13849 = FACE_OUTER_BOUND ( 'NONE', #10656, .T. ) ;
#13850 = FACE_OUTER_BOUND ( 'NONE', #10216, .T. ) ;
#13851 = EDGE_CURVE ( 'NONE', #2753, #3756, #5123, .T. ) ;
#13852 = CARTESIAN_POINT ( 'NONE',  ( 11.79136029199137958, -53.28557117198400306, -4.055532625545659187 ) ) ;
#13853 = CARTESIAN_POINT ( 'NONE',  ( 54.86190032082818391, 1.721056973166403603, 60.61639468829817190 ) ) ;
#13854 = ORIENTED_EDGE ( 'NONE', *, *, #73, .F. ) ;
#13855 = DIRECTION ( 'NONE',  ( -1.000000000000000000, -1.156482317317871725E-16, 0.000000000000000000 ) ) ;
#13856 = DIRECTION ( 'NONE',  ( -1.000000000000000000, 0.000000000000000000, 0.000000000000000000 ) ) ;
#13857 = FACE_OUTER_BOUND ( 'NONE', #9557, .T. ) ;
#13858 = CARTESIAN_POINT ( 'NONE',  ( 54.03086304124234829, 0.8903401505190762233, 62.84860122826521689 ) ) ;
#13859 = DIRECTION ( 'NONE',  ( 1.000000000000000000, 0.000000000000000000, 0.000000000000000000 ) ) ;
#13860 = EDGE_LOOP ( 'NONE', ( #6776, #3142, #2451, #8737 ) ) ;
#13861 = CARTESIAN_POINT ( 'NONE',  ( 69.43919918318417217, -3.018345010862574451, 71.67085758179622701 ) ) ;
#13862 = FACE_OUTER_BOUND ( 'NONE', #9860, .T. ) ;
#13863 = VERTEX_POINT ( 'NONE', #2811 ) ;
#13864 = LINE ( 'NONE', #13023, #4732 ) ;
#13865 = VERTEX_POINT ( 'NONE', #12189 ) ;
#13866 =( NAMED_UNIT ( * ) PLANE_ANGLE_UNIT ( ) SI_UNIT ( $, .RADIAN. ) );
#13867 = CARTESIAN_POINT ( 'NONE',  ( -9.083879796419006780, -7.373836579503426414, -48.00000000000010658 ) ) ;
#13868 = DIRECTION ( 'NONE',  ( 0.8746197071345571672, -0.4848096202550660205, 0.000000000000000000 ) ) ;
#13869 = EDGE_LOOP ( 'NONE', ( #5043, #7069, #12916, #13885 ) ) ;
#13870 = ADVANCED_FACE ( 'NONE', ( #14876, #13883, #15040, #13802, #5343 ), #12497, .F. ) ;
#13871 = DIRECTION ( 'NONE',  ( 0.000000000000000000, -1.000000000000000000, -1.734723475976817547E-15 ) ) ;
#13872 = CYLINDRICAL_SURFACE ( 'NONE', #12843, 10.00000000000000178 ) ;
#13873 = EDGE_CURVE ( 'NONE', #6912, #3132, #6421, .T. ) ;
#13874 = CARTESIAN_POINT ( 'NONE',  ( -16.99999999999998579, -2.249290599286303927, 50.00000000000012079 ) ) ;
#13875 = CARTESIAN_POINT ( 'NONE',  ( 52.35373241494735197, -0.8423457118892125894, 48.51982618741349285 ) ) ;
#13876 = ADVANCED_FACE ( 'NONE', ( #6798 ), #8956, .F. ) ;
#13877 = CARTESIAN_POINT ( 'NONE',  ( -32.80254285330629216, -2.278009980413787439, -57.50000000000012079 ) ) ;
#13878 = CARTESIAN_POINT ( 'NONE',  ( 32.39917484285220439, 23.25070940071368852, -33.00000000000012790 ) ) ;
#13879 = ORIENTED_EDGE ( 'NONE', *, *, #1881, .F. ) ;
#13880 = ORIENTED_EDGE ( 'NONE', *, *, #14128, .T. ) ;
#13881 = CARTESIAN_POINT ( 'NONE',  ( 27.87319062054570296, -68.05254135531041015, -4.069129117103200244 ) ) ;
#13882 = ORIENTED_EDGE ( 'NONE', *, *, #12911, .F. ) ;
#13883 = FACE_BOUND ( 'NONE', #1186, .T. ) ;
#13884 = CARTESIAN_POINT ( 'NONE',  ( 33.12442989620986822, -59.21224831720011395, 1.832439066039631914 ) ) ;
#13885 = ORIENTED_EDGE ( 'NONE', *, *, #487, .T. ) ;
#13886 = DIRECTION ( 'NONE',  ( -0.000000000000000000, -1.000000000000000000, -0.000000000000000000 ) ) ;
#13887 = DIRECTION ( 'NONE',  ( -0.8746197071345569451, 0.4848096202550666312, 0.000000000000000000 ) ) ;
#13888 = DIRECTION ( 'NONE',  ( 1.000000000000000000, 0.000000000000000000, 0.000000000000000000 ) ) ;
#13889 = EDGE_CURVE ( 'NONE', #9584, #3752, #13647, .T. ) ;
#13890 = B_SPLINE_CURVE_WITH_KNOTS ( 'NONE', 3,
 ( #6483, #12331, #11172, #2859 ),
 .UNSPECIFIED., .F., .F.,
 ( 4, 4 ),
 ( 0.006832557018188310620, 0.007799362039380771001 ),
 .UNSPECIFIED. ) ;
#13891 = EDGE_CURVE ( 'NONE', #4611, #6843, #9114, .T. ) ;
#13892 = B_SPLINE_CURVE_WITH_KNOTS ( 'NONE', 3,
 ( #13296, #4042, #1742, #444, #6366, #11201, #14384, #12067, #3825, #7457, #9769, #8532 ),
 .UNSPECIFIED., .F., .F.,
 ( 4, 2, 2, 2, 2, 4 ),
 ( 0.000000000000000000, 0.001071381053236910479, 0.002142762106473820958, 0.003214143159710731654, 0.003749833686329185484, 0.004285524212947640181 ),
 .UNSPECIFIED. ) ;
#13893 = CARTESIAN_POINT ( 'NONE',  ( 76.46532884418532205, -6.768019176512804158, 73.13615421477459222 ) ) ;
#13894 = CARTESIAN_POINT ( 'NONE',  ( -9.456839514482961562, 2.659958822950721835, -57.50000000000012079 ) ) ;
#13895 = FACE_OUTER_BOUND ( 'NONE', #12882, .T. ) ;
#13896 = CARTESIAN_POINT ( 'NONE',  ( 14.30960301864961615, -69.39711819508850965, 4.459166325353795202 ) ) ;
#13897 = CARTESIAN_POINT ( 'NONE',  ( -25.21252699837112132, -6.998437922861946880, -48.50000000000012079 ) ) ;
#13898 = ORIENTED_EDGE ( 'NONE', *, *, #7417, .F. ) ;
#13899 = CARTESIAN_POINT ( 'NONE',  ( 18.10076659936878585, -57.98711502975817211, -6.432599168430029657 ) ) ;
#13900 = VERTEX_POINT ( 'NONE', #792 ) ;
#13901 = CARTESIAN_POINT ( 'NONE',  ( -16.99999999999998579, -12.24929059928630437, 33.00000000000012790 ) ) ;
#13902 = ORIENTED_EDGE ( 'NONE', *, *, #1139, .T. ) ;
#13903 =( LENGTH_UNIT ( ) NAMED_UNIT ( * ) SI_UNIT ( .MILLI., .METRE. ) );
#13904 = DIRECTION ( 'NONE',  ( -1.000000000000000000, 0.000000000000000000, 0.000000000000000000 ) ) ;
#13905 = VECTOR ( 'NONE', #9105, 1000.000000000000000 ) ;
#13906 = CARTESIAN_POINT ( 'NONE',  ( 12.48148056143272377, -64.22824823034756037, -3.135769320951040218 ) ) ;
#13907 = VERTEX_POINT ( 'NONE', #869 ) ;
#13908 = CARTESIAN_POINT ( 'NONE',  ( 82.49066175147797253, 23.25070940071369208, 84.20452624982236500 ) ) ;
#13909 = CARTESIAN_POINT ( 'NONE',  ( 9.025447862944712796, -53.84541978742826274, -3.062363702219679684 ) ) ;
#13910 = CARTESIAN_POINT ( 'NONE',  ( 35.49198652140812982, 21.75070940071315562, 139.1143251403882459 ) ) ;
#13911 = EDGE_CURVE ( 'NONE', #15071, #13411, #3266, .T. ) ;
#13912 = CARTESIAN_POINT ( 'NONE',  ( -80.00000000000001421, -85.24929059928631148, -6.000000000000001776 ) ) ;
#13913 = ORIENTED_EDGE ( 'NONE', *, *, #6926, .F. ) ;
#13914 = ORIENTED_EDGE ( 'NONE', *, *, #1479, .F. ) ;
#13915 =( GEOMETRIC_REPRESENTATION_CONTEXT ( 3 ) GLOBAL_UNCERTAINTY_ASSIGNED_CONTEXT ( ( #1651 ) ) GLOBAL_UNIT_ASSIGNED_CONTEXT ( ( #7097, #168, #10711 ) ) REPRESENTATION_CONTEXT ( 'NONE', 'WORKASPACE' ) );
#13916 = CARTESIAN_POINT ( 'NONE',  ( 0.000000000000000000, 21.75070940071319114, -33.00000000000012790 ) ) ;
#13917 = ORIENTED_EDGE ( 'NONE', *, *, #12483, .T. ) ;
#13918 = CARTESIAN_POINT ( 'NONE',  ( 45.17127246049422240, 0.000000000000000000, -33.00000000000012790 ) ) ;
#13919 = ORIENTED_EDGE ( 'NONE', *, *, #6790, .T. ) ;
#13920 = ORIENTED_EDGE ( 'NONE', *, *, #10106, .T. ) ;
#13921 = LINE ( 'NONE', #4379, #14176 ) ;
#13922 = DIRECTION ( 'NONE',  ( -0.8746197071345572782, 0.4848096202550659650, 0.000000000000000000 ) ) ;
#13923 = ORIENTED_EDGE ( 'NONE', *, *, #10733, .F. ) ;
#13924 = EDGE_CURVE ( 'NONE', #7863, #5141, #14800, .T. ) ;
#13925 = AXIS2_PLACEMENT_3D ( 'NONE', #3130, #3287, #7679 ) ;
#13926 = ADVANCED_FACE ( 'NONE', ( #1804, #4175, #6721 ), #10193, .T. ) ;
#13927 = DIRECTION ( 'NONE',  ( -0.000000000000000000, -0.000000000000000000, -1.000000000000000000 ) ) ;
#13928 = VECTOR ( 'NONE', #796, 1000.000000000000000 ) ;
#13929 = SURFACE_SIDE_STYLE ('',( #6761 ) ) ;
#13930 = ORIENTED_EDGE ( 'NONE', *, *, #7284, .T. ) ;
#13931 = CARTESIAN_POINT ( 'NONE',  ( 80.00000000000001421, -72.24929059928631148, 34.99999999999999289 ) ) ;
#13932 = CARTESIAN_POINT ( 'NONE',  ( 65.13162939515778760, -11.91918766412016772, 73.05968396960713562 ) ) ;
#13933 = CARTESIAN_POINT ( 'NONE',  ( 33.50710080144106229, -55.48278564389710965, -2.668166895089373991 ) ) ;
#13934 = CIRCLE ( 'NONE', #9267, 9.999999999999994671 ) ;
#13935 = DIRECTION ( 'NONE',  ( 0.000000000000000000, 0.000000000000000000, 1.000000000000000000 ) ) ;
#13936 = CARTESIAN_POINT ( 'NONE',  ( 33.43530366116245744, -55.00412896308922939, 2.731447707963691851 ) ) ;
#13937 = ORIENTED_EDGE ( 'NONE', *, *, #14807, .F. ) ;
#13938 = FACE_OUTER_BOUND ( 'NONE', #12579, .T. ) ;
#13939 = EDGE_CURVE ( 'NONE', #14247, #12141, #5947, .T. ) ;
#13940 = ADVANCED_FACE ( 'NONE', ( #8876 ), #4696, .T. ) ;
#13941 = AXIS2_PLACEMENT_3D ( 'NONE', #7190, #3573, #4734 ) ;
#13942 = ORIENTED_EDGE ( 'NONE', *, *, #13939, .T. ) ;
#13943 = CARTESIAN_POINT ( 'NONE',  ( -65.00000000000001421, -85.24929059928629727, -17.47499999999999787 ) ) ;
#13944 = PLANE ( 'NONE',  #8587 ) ;
#13945 = ORIENTED_EDGE ( 'NONE', *, *, #10360, .T. ) ;
#13946 = DIRECTION ( 'NONE',  ( 1.000000000000000000, 0.000000000000000000, 0.000000000000000000 ) ) ;
#13947 = CARTESIAN_POINT ( 'NONE',  ( -9.657039156986668260, -7.465117833064532249, -47.54128347411995037 ) ) ;
#13948 = CARTESIAN_POINT ( 'NONE',  ( 54.00000000000000711, -2.249290599286311032, 36.00000000000012079 ) ) ;
#13949 = ORIENTED_EDGE ( 'NONE', *, *, #388, .F. ) ;
#13950 = EDGE_LOOP ( 'NONE', ( #2737, #11051, #11200, #8425 ) ) ;
#13951 = DIRECTION ( 'NONE',  ( 0.000000000000000000, 0.000000000000000000, 1.000000000000000000 ) ) ;
#13952 = CARTESIAN_POINT ( 'NONE',  ( 33.12442989620986822, -59.21224831720009263, -1.832439066040486120 ) ) ;
#13953 = VECTOR ( 'NONE', #2272, 999.9999999999998863 ) ;
#13954 = VECTOR ( 'NONE', #5490, 1000.000000000000000 ) ;
#13955 = CARTESIAN_POINT ( 'NONE',  ( 10.00023835250150483, -61.42570632716525125, 2.132522520905371977 ) ) ;
#13956 = DIRECTION ( 'NONE',  ( 1.000000000000000000, 0.000000000000000000, -0.000000000000000000 ) ) ;
#13957 = CARTESIAN_POINT ( 'NONE',  ( -65.00000000000001421, -85.27429059928630295, 17.49999999999999645 ) ) ;
#13958 = DIRECTION ( 'NONE',  ( -0.000000000000000000, -1.000000000000000000, -0.000000000000000000 ) ) ;
#13959 = CIRCLE ( 'NONE', #9029, 2.499999999999995115 ) ;
#13960 = ORIENTED_EDGE ( 'NONE', *, *, #11014, .T. ) ;
#13961 = CARTESIAN_POINT ( 'NONE',  ( -16.99999999999998579, 7.750709400713696517, 38.00000000000012079 ) ) ;
#13962 = CIRCLE ( 'NONE', #4359, 10.00000000000000178 ) ;
#13963 = ORIENTED_EDGE ( 'NONE', *, *, #1619, .F. ) ;
#13964 = CARTESIAN_POINT ( 'NONE',  ( 20.86173033120691045, -82.24929059928629727, -3.999999999999999112 ) ) ;
#13965 = CARTESIAN_POINT ( 'NONE',  ( 9.567742742854477456, -53.28162808095388669, 2.408690284354809030 ) ) ;
#13966 = VECTOR ( 'NONE', #3709, 1000.000000000000000 ) ;
#13967 = ORIENTED_EDGE ( 'NONE', *, *, #5512, .T. ) ;
#13968 = CARTESIAN_POINT ( 'NONE',  ( 96.00000000000002842, 6.750709400713692965, -33.00000000000014211 ) ) ;
#13969 = CARTESIAN_POINT ( 'NONE',  ( 50.07597535787931520, -2.249290599286308368, 38.50000000000012790 ) ) ;
#13970 = EDGE_CURVE ( 'NONE', #13900, #13577, #14532, .T. ) ;
#13971 = EDGE_CURVE ( 'NONE', #5118, #7249, #7883, .T. ) ;
#13972 = CARTESIAN_POINT ( 'NONE',  ( -12.33418063572647938, -2.249290599286303927, -50.50000000000012079 ) ) ;
#13973 = LINE ( 'NONE', #7124, #4883 ) ;
#13974 = CYLINDRICAL_SURFACE ( 'NONE', #3707, 0.5000000000000000000 ) ;
#13975 = VECTOR ( 'NONE', #1347, 1000.000000000000000 ) ;
#13976 = DIRECTION ( 'NONE',  ( -0.8656763553492639041, -0.5006040828730973224, -0.000000000000000000 ) ) ;
#13977 = DIRECTION ( 'NONE',  ( 1.000000000000000000, 0.000000000000000000, 0.000000000000000000 ) ) ;
#13978 = VERTEX_POINT ( 'NONE', #14961 ) ;
#13979 = CARTESIAN_POINT ( 'NONE',  ( 9.615492529877293748, -61.48517313030954057, -2.719255632331072370 ) ) ;
#13980 = UNCERTAINTY_MEASURE_WITH_UNIT (LENGTH_MEASURE( 1.000000000000000082E-05 ), #12561, 'distance_accuracy_value', 'NONE');
#13981 = VERTEX_POINT ( 'NONE', #2101 ) ;
#13982 = CARTESIAN_POINT ( 'NONE',  ( -80.00000000000001421, -87.24929059928631148, 35.00000000000000000 ) ) ;
#13983 = EDGE_LOOP ( 'NONE', ( #8775, #6286, #13089, #1426 ) ) ;
#13984 = EDGE_CURVE ( 'NONE', #5864, #9890, #9199, .T. ) ;
#13985 = CARTESIAN_POINT ( 'NONE',  ( 27.49389128939799676, -69.39711819508849544, 4.416273062436605557 ) ) ;
#13986 = CARTESIAN_POINT ( 'NONE',  ( -28.70947653109703168, -9.020656969121420232, -48.00000000000012079 ) ) ;
#13987 = EDGE_CURVE ( 'NONE', #12651, #5130, #3957, .T. ) ;
#13988 = CARTESIAN_POINT ( 'NONE',  ( 16.19211320117534214, -53.25924031079298260, -5.665074923594194622 ) ) ;
#13989 = ORIENTED_EDGE ( 'NONE', *, *, #8623, .F. ) ;
#13990 = DIRECTION ( 'NONE',  ( 0.000000000000000000, 0.000000000000000000, 1.000000000000000000 ) ) ;
#13991 = CARTESIAN_POINT ( 'NONE',  ( 11.09435930935936554, -53.42013688713559816, -3.804487959019770216 ) ) ;
#13992 = DIRECTION ( 'NONE',  ( -0.000000000000000000, -0.000000000000000000, 1.000000000000000000 ) ) ;
#13993 = PLANE ( 'NONE',  #10754 ) ;
#13994 = CIRCLE ( 'NONE', #11519, 3.000000000000002665 ) ;
#13995 = VECTOR ( 'NONE', #5646, 1000.000000000000000 ) ;
#13996 = ORIENTED_EDGE ( 'NONE', *, *, #3417, .F. ) ;
#13997 = ORIENTED_EDGE ( 'NONE', *, *, #1430, .F. ) ;
#13998 = DIRECTION ( 'NONE',  ( 1.000000000000000000, 0.000000000000000000, 0.000000000000000000 ) ) ;
#13999 = ORIENTED_EDGE ( 'NONE', *, *, #10410, .T. ) ;
#14000 = DIRECTION ( 'NONE',  ( 0.000000000000000000, 0.000000000000000000, 1.000000000000000000 ) ) ;
#14001 = ORIENTED_EDGE ( 'NONE', *, *, #13002, .F. ) ;
#14002 = EDGE_CURVE ( 'NONE', #14996, #11430, #1339, .T. ) ;
#14003 = ORIENTED_EDGE ( 'NONE', *, *, #6548, .F. ) ;
#14004 = CARTESIAN_POINT ( 'NONE',  ( -2.688903428702175252E-15, 23.25070940071368142, 33.00000000000012790 ) ) ;
#14005 = DIRECTION ( 'NONE',  ( 0.3738365665314423159, 0.000000000000000000, 0.9274945937977119303 ) ) ;
#14006 = ORIENTED_EDGE ( 'NONE', *, *, #5658, .T. ) ;
#14007 = TOROIDAL_SURFACE ( 'NONE', #7369, 9.500000000000001776, 0.5000000000000000000 ) ;
#14008 = VECTOR ( 'NONE', #1185, 1000.000000000000000 ) ;
#14009 = DIRECTION ( 'NONE',  ( 1.000000000000000000, 0.000000000000000000, 0.000000000000000000 ) ) ;
#14010 = CARTESIAN_POINT ( 'NONE',  ( -16.99999999999998579, -6.754727345143736628, 36.00000000000012079 ) ) ;
#14011 = VERTEX_POINT ( 'NONE', #13964 ) ;
#14012 = CARTESIAN_POINT ( 'NONE',  ( -28.95977857253358323, -8.587818791446789390, 57.50000000000012079 ) ) ;
#14013 = DIRECTION ( 'NONE',  ( 0.000000000000000000, 0.000000000000000000, 1.000000000000000000 ) ) ;
#14014 = DIRECTION ( 'NONE',  ( 1.000000000000000000, 0.000000000000000000, 0.000000000000000000 ) ) ;
#14015 = DIRECTION ( 'NONE',  ( 1.000000000000000000, 0.000000000000000000, -0.000000000000000000 ) ) ;
#14016 = ORIENTED_EDGE ( 'NONE', *, *, #4382, .F. ) ;
#14017 = CARTESIAN_POINT ( 'NONE',  ( 75.52271037289314393, -7.388871293676331220, 72.19766410831374515 ) ) ;
#14018 = AXIS2_PLACEMENT_3D ( 'NONE', #4195, #2902, #6368 ) ;
#14019 = ORIENTED_EDGE ( 'NONE', *, *, #10223, .T. ) ;
#14020 = CARTESIAN_POINT ( 'NONE',  ( -12.99999999999998757, -2.249290599286303483, 38.00000000000012079 ) ) ;
#14021 = CARTESIAN_POINT ( 'NONE',  ( 0.000000000000000000, 0.000000000000000000, 0.000000000000000000 ) ) ;
#14022 = DIRECTION ( 'NONE',  ( -0.000000000000000000, -0.000000000000000000, -1.000000000000000000 ) ) ;
#14023 = CARTESIAN_POINT ( 'NONE',  ( 80.00000000000001421, -72.24929059928631148, 34.99999999999999289 ) ) ;
#14024 = ORIENTED_EDGE ( 'NONE', *, *, #9971, .F. ) ;
#14025 = DIRECTION ( 'NONE',  ( 9.912705577010325549E-17, -1.734723475976817547E-15, 1.000000000000000000 ) ) ;
#14026 = CARTESIAN_POINT ( 'NONE',  ( 31.88156390563087683, -61.30062302791112927, -2.840369378987771753 ) ) ;
#14027 = ADVANCED_FACE ( 'NONE', ( #38 ), #3654, .T. ) ;
#14028 = CIRCLE ( 'NONE', #10803, 3.999999999999999112 ) ;
#14029 = ADVANCED_FACE ( 'NONE', ( #12738 ), #2492, .F. ) ;
#14030 = DIRECTION ( 'NONE',  ( 0.000000000000000000, 1.000000000000000000, 0.000000000000000000 ) ) ;
#14031 = DIRECTION ( 'NONE',  ( 0.000000000000000000, 0.000000000000000000, 1.000000000000000000 ) ) ;
#14032 = CARTESIAN_POINT ( 'NONE',  ( 37.23881781239525424, 23.25070940071368852, -33.00000000000012790 ) ) ;
#14033 = DIRECTION ( 'NONE',  ( 0.000000000000000000, 0.000000000000000000, 1.000000000000000000 ) ) ;
#14034 = PRODUCT_DEFINITION_SHAPE ( 'NONE', 'NONE',  #15231 ) ;
#14035 = EDGE_CURVE ( 'NONE', #11155, #5118, #14056, .T. ) ;
#14036 = EDGE_LOOP ( 'NONE', ( #8742, #6603, #12368, #4428 ) ) ;
#14037 = VECTOR ( 'NONE', #10355, 1000.000000000000000 ) ;
#14038 = DIRECTION ( 'NONE',  ( 0.000000000000000000, 0.000000000000000000, 1.000000000000000000 ) ) ;
#14039 = ORIENTED_EDGE ( 'NONE', *, *, #3194, .F. ) ;
#14040 = CARTESIAN_POINT ( 'NONE',  ( 11.27557984327373575, -52.38203995748321518, -2.900057921394206151 ) ) ;
#14041 = VERTEX_POINT ( 'NONE', #4730 ) ;
#14042 = DIRECTION ( 'NONE',  ( 0.000000000000000000, -0.000000000000000000, 1.000000000000000000 ) ) ;
#14043 = CARTESIAN_POINT ( 'NONE',  ( 80.00000000000001421, -76.24929059928631148, 6.000000000000000000 ) ) ;
#14044 =( LENGTH_UNIT ( ) NAMED_UNIT ( * ) SI_UNIT ( .MILLI., .METRE. ) );
#14045 = AXIS2_PLACEMENT_3D ( 'NONE', #10576, #8193, #4723 ) ;
#14046 = CIRCLE ( 'NONE', #1005, 0.7892041907098286124 ) ;
#14047 = DIRECTION ( 'NONE',  ( 0.000000000000000000, 1.000000000000000000, 0.000000000000000000 ) ) ;
#14048 = CARTESIAN_POINT ( 'NONE',  ( 73.69809405469877106, 29.52935533987996664, -27.49288055531513209 ) ) ;
#14049 = CARTESIAN_POINT ( 'NONE',  ( -25.22031829551916360, -6.987901215495521789, 48.36903577193041315 ) ) ;
#14050 = B_SPLINE_CURVE_WITH_KNOTS ( 'NONE', 3,
 ( #742, #14904, #10376, #4365, #4523, #5452, #10146, #7837, #15075, #13757, #14834, #10300 ),
 .UNSPECIFIED., .F., .F.,
 ( 4, 2, 2, 2, 2, 4 ),
 ( 0.000000000000000000, 0.0002273805472697271570, 0.0004547610945394543139, 0.0009095221890789429971, 0.001364283283618431463, 0.001819044378157920255 ),
 .UNSPECIFIED. ) ;
#14051 = CARTESIAN_POINT ( 'NONE',  ( 23.36173033120691400, -82.24929059928629727, 6.000000000000001776 ) ) ;
#14052 = EDGE_CURVE ( 'NONE', #2307, #13742, #5743, .T. ) ;
#14053 = CARTESIAN_POINT ( 'NONE',  ( 32.05473995880635840, -54.31361072226614084, 3.260388240305548191 ) ) ;
#14054 = ORIENTED_EDGE ( 'NONE', *, *, #2521, .T. ) ;
#14055 = CARTESIAN_POINT ( 'NONE',  ( 9.496763888311855695, -60.90158242453190951, -2.720958400102891250 ) ) ;
#14056 = CIRCLE ( 'NONE', #3724, 0.9999999999999963363 ) ;
#14057 = VECTOR ( 'NONE', #6165, 1000.000000000000000 ) ;
#14058 = EDGE_LOOP ( 'NONE', ( #5777, #14647 ) ) ;
#14059 = CARTESIAN_POINT ( 'NONE',  ( -9.875903985900572835, 2.387222743937554181, 57.50000000000012079 ) ) ;
#14060 =( GEOMETRIC_REPRESENTATION_CONTEXT ( 3 ) GLOBAL_UNCERTAINTY_ASSIGNED_CONTEXT ( ( #9681 ) ) GLOBAL_UNIT_ASSIGNED_CONTEXT ( ( #2863, #12260, #559 ) ) REPRESENTATION_CONTEXT ( 'NONE', 'WORKASPACE' ) );
#14061 = VERTEX_POINT ( 'NONE', #1187 ) ;
#14062 = B_SPLINE_CURVE_WITH_KNOTS ( 'NONE', 3,
 ( #1929, #1852, #1785, #773, #7637, #14709, #14859, #11243, #4238, #12637, #849, #4162, #5488, #3244 ),
 .UNSPECIFIED., .F., .F.,
 ( 4, 2, 2, 2, 2, 2, 4 ),
 ( 8.673617379884035472E-19, 0.002516897397286764395, 0.003775346095930138136, 0.005033794794573512310, 0.006292243493216886051, 0.007550692191860259792, 0.01006758958914700727 ),
 .UNSPECIFIED. ) ;
#14063 = ORIENTED_EDGE ( 'NONE', *, *, #12852, .T. ) ;
#14064 = LINE ( 'NONE', #7208, #5216 ) ;
#14065 = CARTESIAN_POINT ( 'NONE',  ( 35.49198652140812982, 23.25070940071368852, 139.1143251403882459 ) ) ;
#14066 = CARTESIAN_POINT ( 'NONE',  ( 12.02094163398139770, -52.24929059928630437, -4.175384597093463768 ) ) ;
#14067 = VERTEX_POINT ( 'NONE', #12898 ) ;
#14068 = COLOUR_RGB ( '',0.7921568627450980005, 0.8196078431372548767, 0.9333333333333333481 ) ;
#14069 = VERTEX_POINT ( 'NONE', #4881 ) ;
#14070 = VECTOR ( 'NONE', #7807, 1000.000000000000000 ) ;
#14071 = AXIS2_PLACEMENT_3D ( 'NONE', #11936, #2480, #6029 ) ;
#14072 = DIRECTION ( 'NONE',  ( -1.000000000000000000, 0.000000000000000000, 0.000000000000000000 ) ) ;
#14073 = EDGE_CURVE ( 'NONE', #12316, #6772, #1101, .T. ) ;
#14074 = EDGE_CURVE ( 'NONE', #3807, #14139, #6004, .T. ) ;
#14075 = CYLINDRICAL_SURFACE ( 'NONE', #433, 3.000000000000000000 ) ;
#14076 = AXIS2_PLACEMENT_3D ( 'NONE', #7303, #12150, #11060 ) ;
#14077 = VERTEX_POINT ( 'NONE', #2186 ) ;
#14078 = ORIENTED_EDGE ( 'NONE', *, *, #5898, .T. ) ;
#14079 = CARTESIAN_POINT ( 'NONE',  ( 0.000000000000000000, 21.75070940071329417, -33.00000000000012790 ) ) ;
#14080 = VERTEX_POINT ( 'NONE', #13042 ) ;
#14081 = DIRECTION ( 'NONE',  ( 0.4848096202550659650, 0.8746197071345572782, -0.000000000000000000 ) ) ;
#14082 = VERTEX_POINT ( 'NONE', #15194 ) ;
#14083 = EDGE_LOOP ( 'NONE', ( #13381, #12963, #12317, #5877 ) ) ;
#14084 = CARTESIAN_POINT ( 'NONE',  ( 67.21328690825529861, 29.52935533987996664, -21.00807340887166674 ) ) ;
#14085 = CARTESIAN_POINT ( 'NONE',  ( 43.00000000000000711, 10.25070940071368497, -33.00000000000012790 ) ) ;
#14086 = ORIENTED_EDGE ( 'NONE', *, *, #13851, .F. ) ;
#14087 = AXIS2_PLACEMENT_3D ( 'NONE', #9832, #8727, #14512 ) ;
#14088 = CARTESIAN_POINT ( 'NONE',  ( 68.02719294894561131, -7.807454411681060691, 61.61639468829817190 ) ) ;
#14089 = CARTESIAN_POINT ( 'NONE',  ( -65.00000000000001421, -85.24929059928631148, 22.52499999999999503 ) ) ;
#14090 = EDGE_LOOP ( 'NONE', ( #10343, #225, #8812, #4488 ) ) ;
#14091 = ADVANCED_FACE ( 'NONE', ( #8200 ), #7034, .T. ) ;
#14092 = LINE ( 'NONE', #12788, #8771 ) ;
#14093 = DIRECTION ( 'NONE',  ( 0.000000000000000000, 0.000000000000000000, -1.000000000000000000 ) ) ;
#14094 = EDGE_CURVE ( 'NONE', #9073, #3836, #14119, .T. ) ;
#14095 = DIRECTION ( 'NONE',  ( 1.000000000000000000, 0.000000000000000000, 0.000000000000000000 ) ) ;
#14096 = ORIENTED_EDGE ( 'NONE', *, *, #9974, .T. ) ;
#14097 = AXIS2_PLACEMENT_3D ( 'NONE', #14836, #11149, #12448 ) ;
#14098 = CARTESIAN_POINT ( 'NONE',  ( 70.18619815789806182, -3.934114537491368857, 72.29468792547720568 ) ) ;
#14099 = AXIS2_PLACEMENT_3D ( 'NONE', #14246, #7236, #4930 ) ;
#14100 = ORIENTED_EDGE ( 'NONE', *, *, #6089, .T. ) ;
#14101 = FACE_OUTER_BOUND ( 'NONE', #906, .T. ) ;
#14102 = FACE_OUTER_BOUND ( 'NONE', #2321, .T. ) ;
#14103 = DIRECTION ( 'NONE',  ( 0.000000000000000000, 0.000000000000000000, 1.000000000000000000 ) ) ;
#14104 = CARTESIAN_POINT ( 'NONE',  ( -10.08688311991301312, -8.022742138608869311, -47.66502101098957667 ) ) ;
#14105 = CARTESIAN_POINT ( 'NONE',  ( 62.14609464170151654, 0.6526447315840442354, 62.84860122826521689 ) ) ;
#14106 = ORIENTED_EDGE ( 'NONE', *, *, #7774, .F. ) ;
#14107 = ORIENTED_EDGE ( 'NONE', *, *, #8044, .T. ) ;
#14108 = CARTESIAN_POINT ( 'NONE',  ( -9.456839502978525047, 2.659958805273927140, -48.36906329404666849 ) ) ;
#14109 = PLANE ( 'NONE',  #7379 ) ;
#14110 = DIRECTION ( 'NONE',  ( -0.000000000000000000, 0.000000000000000000, 1.000000000000000000 ) ) ;
#14111 = DIRECTION ( 'NONE',  ( -0.000000000000000000, 0.000000000000000000, -1.000000000000000000 ) ) ;
#14112 = CARTESIAN_POINT ( 'NONE',  ( -3.285520523749251520, 5.681530634151883419, 48.00000000000012079 ) ) ;
#14113 = LINE ( 'NONE', #3565, #13308 ) ;
#14114 = EDGE_CURVE ( 'NONE', #8236, #13054, #118, .T. ) ;
#14115 = EDGE_LOOP ( 'NONE', ( #6508, #9413, #12535, #7885 ) ) ;
#14116 = DIRECTION ( 'NONE',  ( 1.000000000000000000, 0.000000000000000000, 0.000000000000000000 ) ) ;
#14117 = ORIENTED_EDGE ( 'NONE', *, *, #3201, .T. ) ;
#14118 = EDGE_CURVE ( 'NONE', #1907, #13470, #4961, .T. ) ;
#14119 = LINE ( 'NONE', #8275, #9391 ) ;
#14120 = CARTESIAN_POINT ( 'NONE',  ( 118.2606911748681568, -35.65233716510192608, 53.46824312087640863 ) ) ;
#14121 = VERTEX_POINT ( 'NONE', #7336 ) ;
#14122 = EDGE_CURVE ( 'NONE', #943, #11350, #2574, .T. ) ;
#14123 = LINE ( 'NONE', #1413, #4491 ) ;
#14124 = CARTESIAN_POINT ( 'NONE',  ( 53.45023817967523172, -5.433760736713491468, 54.56811043785582882 ) ) ;
#14125 = DIRECTION ( 'NONE',  ( 0.000000000000000000, 0.000000000000000000, 1.000000000000000000 ) ) ;
#14126 = DIRECTION ( 'NONE',  ( -1.000000000000000000, -0.000000000000000000, -0.000000000000000000 ) ) ;
#14127 = ADVANCED_FACE ( 'NONE', ( #8708 ), #8426, .F. ) ;
#14128 = EDGE_CURVE ( 'NONE', #619, #5990, #11094, .T. ) ;
#14129 = DIRECTION ( 'NONE',  ( 0.000000000000000000, 1.734723475976817547E-15, -1.000000000000000000 ) ) ;
#14130 = FACE_OUTER_BOUND ( 'NONE', #6540, .T. ) ;
#14131 = CARTESIAN_POINT ( 'NONE',  ( -24.83354747574476207, -6.700581361908810152, 48.23896987259369240 ) ) ;
#14132 = DIRECTION ( 'NONE',  ( -1.000000000000000000, -8.673617379884035472E-17, 0.000000000000000000 ) ) ;
#14133 = CARTESIAN_POINT ( 'NONE',  ( 32.21946295013410122, -53.34604504765228938, 2.388784160329073814 ) ) ;
#14134 = ORIENTED_EDGE ( 'NONE', *, *, #937, .T. ) ;
#14135 = DIRECTION ( 'NONE',  ( 0.000000000000000000, 1.000000000000000000, -0.000000000000000000 ) ) ;
#14136 = ORIENTED_EDGE ( 'NONE', *, *, #8610, .T. ) ;
#14137 = ADVANCED_FACE ( 'NONE', ( #4956 ), #8157, .F. ) ;
#14138 = DIRECTION ( 'NONE',  ( 0.8381289428352243220, 0.5454721580263371949, 0.000000000000000000 ) ) ;
#14139 = VERTEX_POINT ( 'NONE', #2717 ) ;
#14140 = EDGE_CURVE ( 'NONE', #1580, #5593, #14422, .T. ) ;
#14141 = ORIENTED_EDGE ( 'NONE', *, *, #9176, .T. ) ;
#14142 = CARTESIAN_POINT ( 'NONE',  ( 65.33089625181217741, -11.07072041448327226, 76.23223904883872137 ) ) ;
#14143 = CARTESIAN_POINT ( 'NONE',  ( 96.29968967959054282, 23.25070940071369208, 84.20452624982236500 ) ) ;
#14144 =( BOUNDED_SURFACE ( )  B_SPLINE_SURFACE ( 3, 2, ( 
 ( #5416, #12187, #4023 ),
 ( #567, #10968, #2728 ),
 ( #8797, #4098, #1720 ),
 ( #11181, #8718, #2959 ),
 ( #7652, #13279, #5119 ),
 ( #6277, #1864, #12122 ),
 ( #1801, #420, #7573 ),
 ( #6492, #5269, #9823 ),
 ( #12266, #632, #5340 ),
 ( #9964, #3950, #8649 ),
 ( #10190, #10342, #4568 ),
 ( #8954, #867, #3335 ),
 ( #7881, #13881, #10426 ),
 ( #15117, #12735, #9197 ) ),
 .UNSPECIFIED., .F., .F., .F. ) 
 B_SPLINE_SURFACE_WITH_KNOTS ( ( 4, 2, 2, 2, 2, 2, 4 ),
 ( 3, 3 ),
 ( 0.2948322565876199119, 0.2981287057529276030, 0.3014251549182353496, 0.3080180532488507872, 0.3146109515794662803, 0.3179074007447739714, 0.3212038499100817179 ),
 ( 0.000000000000000000, 0.9256633218932677210 ),
 .UNSPECIFIED. ) 
 GEOMETRIC_REPRESENTATION_ITEM ( )  RATIONAL_B_SPLINE_SURFACE ( (
 ( 1.000000000000000000, 0.9979219307738474987, 0.9996910464737041035),
 ( 1.000000000000000000, 0.9979571442240253720, 0.9996962817755257191),
 ( 1.000000000000000000, 0.9979896195972790540, 0.9997011099982617832),
 ( 1.000000000000000000, 0.9980478678146850191, 0.9997097699562369488),
 ( 1.000000000000000000, 0.9980736641738252590, 0.9997136051875283869),
 ( 1.000000000000000000, 0.9981411222207057232, 0.9997236344017617071),
 ( 1.000000000000000000, 0.9981728461537401342, 0.9997283509053582762),
 ( 1.000000000000000000, 0.9982102196780588965, 0.9997339073526521069),
 ( 1.000000000000000000, 0.9982158677593770957, 0.9997347470718578322),
 ( 1.000000000000000000, 0.9982052731646248178, 0.9997331719378983461),
 ( 1.000000000000000000, 0.9981985596398339489, 0.9997321738156357274),
 ( 1.000000000000000000, 0.9981789131846819929, 0.9997292529112105086),
 ( 1.000000000000000000, 0.9981660722458856050, 0.9997273438057427963),
 ( 1.000000000000000000, 0.9981504490785558792, 0.9997250210570212126) ) ) 
 REPRESENTATION_ITEM ( '' )  SURFACE ( )  );
#14145 = CARTESIAN_POINT ( 'NONE',  ( 80.00000000000001421, -87.24929059928631148, 35.00000000000000000 ) ) ;
#14146 = CARTESIAN_POINT ( 'NONE',  ( 8.996939472011559857, -55.34955111272346784, 2.958349455637744541 ) ) ;
#14147 = CARTESIAN_POINT ( 'NONE',  ( 9.200644618036294631, -59.06479067038042530, -2.757123406423244383 ) ) ;
#14148 = CARTESIAN_POINT ( 'NONE',  ( 80.00000000000001421, -74.24929059928631148, -32.99999999999999289 ) ) ;
#14149 = FACE_OUTER_BOUND ( 'NONE', #14601, .T. ) ;
#14150 = ORIENTED_EDGE ( 'NONE', *, *, #8146, .F. ) ;
#14151 = ORIENTED_EDGE ( 'NONE', *, *, #6409, .T. ) ;
#14152 = CARTESIAN_POINT ( 'NONE',  ( 64.20382552624532480, -11.89050466264470529, 75.84179418424443497 ) ) ;
#14153 = VERTEX_POINT ( 'NONE', #9664 ) ;
#14154 = CARTESIAN_POINT ( 'NONE',  ( 0.9298897195970434737, -1.451567674087680837, -48.00000000000012079 ) ) ;
#14155 = ORIENTED_EDGE ( 'NONE', *, *, #12428, .T. ) ;
#14156 = CARTESIAN_POINT ( 'NONE',  ( 16.17808712816582783, -52.24929059928630437, 5.670202843280253369 ) ) ;
#14157 = AXIS2_PLACEMENT_3D ( 'NONE', #3250, #9185, #4557 ) ;
#14158 = ORIENTED_EDGE ( 'NONE', *, *, #11767, .T. ) ;
#14159 = CARTESIAN_POINT ( 'NONE',  ( -12.99999999999998757, -2.249290599286158709, 33.00000000000012790 ) ) ;
#14160 = DIRECTION ( 'NONE',  ( 0.000000000000000000, 0.000000000000000000, 1.000000000000000000 ) ) ;
#14161 = ORIENTED_EDGE ( 'NONE', *, *, #2967, .T. ) ;
#14162 = EDGE_CURVE ( 'NONE', #14011, #10151, #5448, .T. ) ;
#14163 = CARTESIAN_POINT ( 'NONE',  ( 118.0000000000000284, 19.25070940071370273, 13.14990448602693007 ) ) ;
#14164 = DIRECTION ( 'NONE',  ( 0.000000000000000000, 0.000000000000000000, 1.000000000000000000 ) ) ;
#14165 = ORIENTED_EDGE ( 'NONE', *, *, #12183, .T. ) ;
#14166 = VECTOR ( 'NONE', #8023, 1000.000000000000000 ) ;
#14167 = CARTESIAN_POINT ( 'NONE',  ( 80.18290120114222930, 23.25070940071369208, -33.00000000000012790 ) ) ;
#14168 = LINE ( 'NONE', #13246, #10352 ) ;
#14169 = DIRECTION ( 'NONE',  ( 0.000000000000000000, -1.000000000000000000, 0.000000000000000000 ) ) ;
#14170 = VERTEX_POINT ( 'NONE', #405 ) ;
#14171 = MANIFOLD_SOLID_BREP ( 'Body-Move/Copy1', #5298 ) ;
#14172 = CARTESIAN_POINT ( 'NONE',  ( -24.72817752516935741, 2.363221963240438761, 48.00000000000019185 ) ) ;
#14173 = VERTEX_POINT ( 'NONE', #13188 ) ;
#14174 = PLANE ( 'NONE',  #5203 ) ;
#14175 = DIRECTION ( 'NONE',  ( 0.000000000000000000, 0.000000000000000000, 1.000000000000000000 ) ) ;
#14176 = VECTOR ( 'NONE', #14845, 1000.000000000000000 ) ;
#14177 = VERTEX_POINT ( 'NONE', #2643 ) ;
#14178 = EDGE_CURVE ( 'NONE', #9131, #1671, #14492, .T. ) ;
#14179 = VECTOR ( 'NONE', #4432, 1000.000000000000000 ) ;
#14180 = EDGE_CURVE ( 'NONE', #13135, #14170, #3965, .T. ) ;
#14181 = CARTESIAN_POINT ( 'NONE',  ( 0.000000000000000000, 0.000000000000000000, 0.000000000000000000 ) ) ;
#14182 = FACE_OUTER_BOUND ( 'NONE', #12927, .T. ) ;
#14183 = DIRECTION ( 'NONE',  ( 0.000000000000000000, -0.000000000000000000, -1.000000000000000000 ) ) ;
#14184 = CARTESIAN_POINT ( 'NONE',  ( -26.99999999999998934, -2.249290599286302150, 33.00000000000009948 ) ) ;
#14185 = DIRECTION ( 'NONE',  ( -1.387778780781444413E-14, 1.127570259384923665E-14, -1.000000000000000000 ) ) ;
#14186 = VECTOR ( 'NONE', #1158, 1000.000000000000000 ) ;
#14187 = CARTESIAN_POINT ( 'NONE',  ( -3.190546569013415379, 0.8906624217387615339, 48.00000000000012079 ) ) ;
#14188 = CYLINDRICAL_SURFACE ( 'NONE', #7362, 0.7892041907098261699 ) ;
#14189 = CARTESIAN_POINT ( 'NONE',  ( 33.44446161014174379, -55.23290567775144666, 1.966731800905200833 ) ) ;
#14190 = CIRCLE ( 'NONE', #6320, 9.000000000000001776 ) ;
#14191 = CARTESIAN_POINT ( 'NONE',  ( 33.31720230358228463, -54.90785108970916184, -2.018552575027052765 ) ) ;
#14192 = CIRCLE ( 'NONE', #5582, 3.999999999999999112 ) ;
#14193 = ORIENTED_EDGE ( 'NONE', *, *, #11099, .F. ) ;
#14194 = ORIENTED_EDGE ( 'NONE', *, *, #4232, .T. ) ;
#14195 = CARTESIAN_POINT ( 'NONE',  ( 58.00000000000000711, -2.249290599286309256, 61.61639468829817190 ) ) ;
#14196 = ORIENTED_EDGE ( 'NONE', *, *, #2754, .T. ) ;
#14197 = CARTESIAN_POINT ( 'NONE',  ( 8.091875466796944139, -56.52532528994184702, -1.842181053809134994 ) ) ;
#14198 = CARTESIAN_POINT ( 'NONE',  ( 56.25419740419757630, 3.022649838004307199, 54.56811043785582882 ) ) ;
#14199 = CIRCLE ( 'NONE', #704, 0.9999999999999991118 ) ;
#14200 = MANIFOLD_SOLID_BREP ( 'Boss-Extrude16', #8786 ) ;
#14201 = CARTESIAN_POINT ( 'NONE',  ( 88.00000000000001421, 10.75070940071369208, 84.20452624982236500 ) ) ;
#14202 = DIRECTION ( 'NONE',  ( 0.000000000000000000, 0.000000000000000000, -1.000000000000000000 ) ) ;
#14203 = AXIS2_PLACEMENT_3D ( 'NONE', #9398, #12941, #2151 ) ;
#14204 = AXIS2_PLACEMENT_3D ( 'NONE', #3940, #1787, #13559 ) ;
#14205 = CARTESIAN_POINT ( 'NONE',  ( 65.00000000000001421, -85.24929059928631148, 22.52499999999999503 ) ) ;
#14206 = CARTESIAN_POINT ( 'NONE',  ( 64.46753801043549004, -11.71576859601145593, 71.98115573486096253 ) ) ;
#14207 = CARTESIAN_POINT ( 'NONE',  ( -80.00000000000001421, -87.24929059928631148, -35.00000000000000000 ) ) ;
#14208 = CARTESIAN_POINT ( 'NONE',  ( -24.55671735758753726, -7.137878559097176279, 48.23807154671105479 ) ) ;
#14209 = CIRCLE ( 'NONE', #11004, 4.505436745857433145 ) ;
#14210 = CARTESIAN_POINT ( 'NONE',  ( 32.56422413728613918, -55.01088356445131211, 3.038469202939856562 ) ) ;
#14211 = EDGE_LOOP ( 'NONE', ( #2560, #6481, #15058, #11980 ) ) ;
#14212 = VECTOR ( 'NONE', #10948, 1000.000000000000000 ) ;
#14213 = CARTESIAN_POINT ( 'NONE',  ( 114.6731053250840233, 21.75070940071369918, -13.14990448602693007 ) ) ;
#14214 = ORIENTED_EDGE ( 'NONE', *, *, #6815, .F. ) ;
#14215 = EDGE_CURVE ( 'NONE', #1809, #11258, #9738, .T. ) ;
#14216 = CARTESIAN_POINT ( 'NONE',  ( 108.0866310645538562, 0.000000000000000000, 13.14990448602693007 ) ) ;
#14217 = ORIENTED_EDGE ( 'NONE', *, *, #1739, .T. ) ;
#14218 = CARTESIAN_POINT ( 'NONE',  ( 65.51024544200237187, -10.91545772570538553, 76.25780573704503240 ) ) ;
#14219 = DIRECTION ( 'NONE',  ( 0.000000000000000000, 0.000000000000000000, 1.000000000000000000 ) ) ;
#14220 = CARTESIAN_POINT ( 'NONE',  ( 61.18622467607353599, 2.299242679852278481, 60.61639468829817190 ) ) ;
#14221 = AXIS2_PLACEMENT_3D ( 'NONE', #12702, #10472, #12872 ) ;
#14222 = CARTESIAN_POINT ( 'NONE',  ( 9.277478075084694353, -53.56578013995677168, 2.318572182806073023 ) ) ;
#14223 = EDGE_CURVE ( 'NONE', #9231, #4765, #14062, .T. ) ;
#14224 = EDGE_CURVE ( 'NONE', #13251, #8699, #6682, .T. ) ;
#14225 = DIRECTION ( 'NONE',  ( 0.000000000000000000, 0.000000000000000000, 1.000000000000000000 ) ) ;
#14226 = CARTESIAN_POINT ( 'NONE',  ( -65.00000000000001421, -85.27429059928628874, -22.50000000000000000 ) ) ;
#14227 = ORIENTED_EDGE ( 'NONE', *, *, #1969, .F. ) ;
#14228 = VERTEX_POINT ( 'NONE', #8860 ) ;
#14229 = DIRECTION ( 'NONE',  ( 0.000000000000000000, 0.000000000000000000, -1.000000000000000000 ) ) ;
#14230 = ORIENTED_EDGE ( 'NONE', *, *, #6742, .F. ) ;
#14231 = CARTESIAN_POINT ( 'NONE',  ( 56.13062797998802722, -6.952138427283281352, 62.84860122826521689 ) ) ;
#14232 = ORIENTED_EDGE ( 'NONE', *, *, #13784, .T. ) ;
#14233 = CARTESIAN_POINT ( 'NONE',  ( 67.21328690825531282, 22.43695620243006772, 84.20452624982236500 ) ) ;
#14234 = CIRCLE ( 'NONE', #12015, 4.665819364273509073 ) ;
#14235 = VERTEX_POINT ( 'NONE', #6703 ) ;
#14236 = CARTESIAN_POINT ( 'NONE',  ( 58.00000000000000711, 10.75070940071368852, 33.00000000000012790 ) ) ;
#14237 = DIRECTION ( 'NONE',  ( -0.8746197071345572782, 0.4848096202550659650, 0.000000000000000000 ) ) ;
#14238 = EDGE_LOOP ( 'NONE', ( #427, #14833, #2010, #12839 ) ) ;
#14239 = CARTESIAN_POINT ( 'NONE',  ( 27.25620696618383221, -52.24929059928630437, -3.946667064627065180 ) ) ;
#14240 = DIRECTION ( 'NONE',  ( 0.4848096202550659650, 0.8746197071345572782, -0.000000000000000000 ) ) ;
#14241 = VERTEX_POINT ( 'NONE', #12479 ) ;
#14242 = CIRCLE ( 'NONE', #952, 0.5000000000000004441 ) ;
#14243 = DIRECTION ( 'NONE',  ( -0.000000000000000000, -0.000000000000000000, -1.000000000000000000 ) ) ;
#14244 = CARTESIAN_POINT ( 'NONE',  ( -9.215065577852303846, 2.268247386559545387, -47.63220435834860922 ) ) ;
#14245 = APPLICATION_CONTEXT ( 'automotive_design' ) ;
#14246 = CARTESIAN_POINT ( 'NONE',  ( 54.03086304124234829, 0.8903401505190762233, 48.51982618741349285 ) ) ;
#14247 = VERTEX_POINT ( 'NONE', #6777 ) ;
#14248 = CARTESIAN_POINT ( 'NONE',  ( -5.290523468902621929, 4.522075770548486418, 57.50000000000012079 ) ) ;
#14249 = EDGE_CURVE ( 'NONE', #1508, #1111, #8890, .T. ) ;
#14250 = EDGE_LOOP ( 'NONE', ( #6437, #1023, #1617, #317 ) ) ;
#14251 = FACE_OUTER_BOUND ( 'NONE', #1381, .T. ) ;
#14252 = AXIS2_PLACEMENT_3D ( 'NONE', #12874, #9172, #13859 ) ;
#14253 = DIRECTION ( 'NONE',  ( -0.000000000000000000, 1.000000000000000000, 1.445602896647339163E-16 ) ) ;
#14254 = AXIS2_PLACEMENT_3D ( 'NONE', #6412, #9961, #13566 ) ;
#14255 = EDGE_LOOP ( 'NONE', ( #8271, #13930, #12968, #7157 ) ) ;
#14256 =( LENGTH_UNIT ( ) NAMED_UNIT ( * ) SI_UNIT ( .MILLI., .METRE. ) );
#14257 = LINE ( 'NONE', #10638, #11238 ) ;
#14258 = DIRECTION ( 'NONE',  ( 0.8208219420614746298, -0.4549890321264247195, -0.3453061251630045736 ) ) ;
#14259 = CYLINDRICAL_SURFACE ( 'NONE', #14884, 0.5000000000000002220 ) ;
#14260 = PLANE ( 'NONE',  #6874 ) ;
#14261 = CARTESIAN_POINT ( 'NONE',  ( 20.86173033120691045, -96.56299909827106376, -3.999999999999999112 ) ) ;
#14262 = CARTESIAN_POINT ( 'NONE',  ( 27.80982499094064408, -66.07496666188232837, 4.402666029760359478 ) ) ;
#14263 = DIRECTION ( 'NONE',  ( 0.3020115420618164626, -0.1674077314120084592, 0.9384901064608666132 ) ) ;
#14264 = AXIS2_PLACEMENT_3D ( 'NONE', #4894, #1202, #208 ) ;
#14265 = CARTESIAN_POINT ( 'NONE',  ( 32.13731150908262180, -54.40375996999018327, -3.226241354721974819 ) ) ;
#14266 = EDGE_CURVE ( 'NONE', #11670, #8958, #13556, .T. ) ;
#14267 = EDGE_CURVE ( 'NONE', #7109, #9216, #11465, .T. ) ;
#14268 = CARTESIAN_POINT ( 'NONE',  ( 9.200644618036296407, -59.06479067038043240, -2.757123406423053424 ) ) ;
#14269 = ORIENTED_EDGE ( 'NONE', *, *, #753, .T. ) ;
#14270 = DIRECTION ( 'NONE',  ( -0.000000000000000000, -0.000000000000000000, -1.000000000000000000 ) ) ;
#14271 = LINE ( 'NONE', #3719, #6936 ) ;
#14272 = ORIENTED_EDGE ( 'NONE', *, *, #2036, .F. ) ;
#14273 = FACE_OUTER_BOUND ( 'NONE', #9621, .T. ) ;
#14274 = DIRECTION ( 'NONE',  ( -0.000000000000000000, -0.000000000000000000, 1.000000000000000000 ) ) ;
#14275 = CARTESIAN_POINT ( 'NONE',  ( 80.00000000000001421, -76.24929059928631148, -4.000000000000000000 ) ) ;
#14276 = CARTESIAN_POINT ( 'NONE',  ( -3.285520523750506516, 5.681530634152946568, -48.50000000000012079 ) ) ;
#14277 = DIRECTION ( 'NONE',  ( 1.000000000000000000, 0.000000000000000000, 0.000000000000000000 ) ) ;
#14278 = CARTESIAN_POINT ( 'NONE',  ( -25.32021674380207799, -6.838035406461215437, 48.10016682092218332 ) ) ;
#14279 = EDGE_CURVE ( 'NONE', #5382, #11723, #13327, .T. ) ;
#14280 = TOROIDAL_SURFACE ( 'NONE', #9124, 9.500000000000001776, 0.5000000000000000000 ) ;
#14281 = CARTESIAN_POINT ( 'NONE',  ( 29.97935572506992230, -52.28363178956111312, 3.029531835800513218 ) ) ;
#14282 = ORIENTED_EDGE ( 'NONE', *, *, #11952, .T. ) ;
#14283 = CARTESIAN_POINT ( 'NONE',  ( 60.05137561479872232, 2.911430354694811484, 54.56811043785582882 ) ) ;
#14284 = EDGE_LOOP ( 'NONE', ( #2981, #12599, #1516, #13629 ) ) ;
#14285 = FACE_OUTER_BOUND ( 'NONE', #7825, .T. ) ;
#14286 = VERTEX_POINT ( 'NONE', #695 ) ;
#14287 = CIRCLE ( 'NONE', #13096, 1.000000000000001110 ) ;
#14288 = CARTESIAN_POINT ( 'NONE',  ( 58.00000000000000711, -2.249290599286309256, 86.40005259842790508 ) ) ;
#14289 = CARTESIAN_POINT ( 'NONE',  ( 58.00000000000000711, -2.249290599286309256, 39.50000000000012790 ) ) ;
#14290 = CIRCLE ( 'NONE', #12812, 0.5000000000000004441 ) ;
#14291 = FACE_OUTER_BOUND ( 'NONE', #9228, .T. ) ;
#14292 = MANIFOLD_SOLID_BREP ( 'Boss-Extrude17', #4565 ) ;
#14293 = CARTESIAN_POINT ( 'NONE',  ( 8.872946762439195112, -55.70527662866908969, 2.889323894642001012 ) ) ;
#14294 = CARTESIAN_POINT ( 'NONE',  ( -24.65452791727695114, 3.133494033999976391, 48.02161282446748203 ) ) ;
#14295 = CIRCLE ( 'NONE', #9133, 31.00000000000000000 ) ;
#14296 = AXIS2_PLACEMENT_3D ( 'NONE', #6517, #596, #11143 ) ;
#14297 = DIRECTION ( 'NONE',  ( -1.000000000000000000, -1.156482317317870492E-16, 0.000000000000000000 ) ) ;
#14298 = EDGE_LOOP ( 'NONE', ( #9285, #10845, #12246, #7304, #11501, #4529, #13667 ) ) ;
#14299 = VECTOR ( 'NONE', #11717, 1000.000000000000000 ) ;
#14300 = ORIENTED_EDGE ( 'NONE', *, *, #3154, .T. ) ;
#14301 = CARTESIAN_POINT ( 'NONE',  ( 0.000000000000000000, 21.75070940071356418, -33.00000000000012790 ) ) ;
#14302 = EDGE_CURVE ( 'NONE', #4834, #358, #5404, .T. ) ;
#14303 = ORIENTED_EDGE ( 'NONE', *, *, #9520, .T. ) ;
#14304 = CARTESIAN_POINT ( 'NONE',  ( 65.00000000000001421, -87.24929059928631148, 22.49999999999999289 ) ) ;
#14305 = ORIENTED_EDGE ( 'NONE', *, *, #4997, .F. ) ;
#14306 = CARTESIAN_POINT ( 'NONE',  ( 31.88156390563088038, -61.30062302791114348, 2.840369378987781968 ) ) ;
#14307 = VERTEX_POINT ( 'NONE', #12950 ) ;
#14308 = ADVANCED_FACE ( 'NONE', ( #2399 ), #11703, .F. ) ;
#14309 = EDGE_CURVE ( 'NONE', #166, #7863, #7096, .T. ) ;
#14310 = ADVANCED_FACE ( 'NONE', ( #14101 ), #5949, .T. ) ;
#14311 = VECTOR ( 'NONE', #14546, 1000.000000000000000 ) ;
#14312 = DIRECTION ( 'NONE',  ( 0.000000000000000000, -1.000000000000000000, -1.734723475976817744E-15 ) ) ;
#14313 = DIRECTION ( 'NONE',  ( 0.000000000000000000, 1.000000000000000000, 0.000000000000000000 ) ) ;
#14314 = ORIENTED_EDGE ( 'NONE', *, *, #2478, .F. ) ;
#14315 = CIRCLE ( 'NONE', #10631, 3.999999999999999112 ) ;
#14316 = MECHANICAL_DESIGN_GEOMETRIC_PRESENTATION_REPRESENTATION (  '', ( #533 ), #14060 ) ;
#14317 = CARTESIAN_POINT ( 'NONE',  ( 108.0866310645538562, 0.000000000000000000, -13.14990448602693007 ) ) ;
#14318 = DIRECTION ( 'NONE',  ( -1.734723475976807292E-15, 1.000000000000000000, 0.000000000000000000 ) ) ;
#14319 = ORIENTED_EDGE ( 'NONE', *, *, #4323, .F. ) ;
#14320 = EDGE_CURVE ( 'NONE', #12939, #6522, #10479, .T. ) ;
#14321 = DIRECTION ( 'NONE',  ( -0.000000000000000000, 1.000000000000000000, -0.000000000000000000 ) ) ;
#14322 = CARTESIAN_POINT ( 'NONE',  ( -9.037775043065352065, 2.932694901963889489, -58.00000000000012079 ) ) ;
#14323 = CARTESIAN_POINT ( 'NONE',  ( 0.5043391135745837195, 0.8906624217387615339, -48.00000000000012079 ) ) ;
#14324 = ORIENTED_EDGE ( 'NONE', *, *, #14807, .T. ) ;
#14325 = PRESENTATION_LAYER_ASSIGNMENT (  '', '', ( #11112 ) ) ;
#14326 = CARTESIAN_POINT ( 'NONE',  ( -25.15752072101216896, 2.619472661158628313, 48.00000000000012079 ) ) ;
#14327 = VECTOR ( 'NONE', #11685, 1000.000000000000000 ) ;
#14328 = CIRCLE ( 'NONE', #2526, 0.7892041907098262810 ) ;
#14329 = ORIENTED_EDGE ( 'NONE', *, *, #9037, .T. ) ;
#14330 = AXIS2_PLACEMENT_3D ( 'NONE', #543, #7629, #12251 ) ;
#14331 = FACE_OUTER_BOUND ( 'NONE', #10997, .T. ) ;
#14332 = CARTESIAN_POINT ( 'NONE',  ( 54.86190032082818391, 1.721056973166403603, 48.51982618741349285 ) ) ;
#14333 = ORIENTED_EDGE ( 'NONE', *, *, #3153, .F. ) ;
#14334 = ADVANCED_FACE ( 'NONE', ( #4472 ), #3631, .T. ) ;
#14335 = B_SPLINE_CURVE_WITH_KNOTS ( 'NONE', 3,
 ( #6952, #13392, #5028, #9873, #2850, #2935, #6261, #11084 ),
 .UNSPECIFIED., .F., .F.,
 ( 4, 2, 2, 4 ),
 ( 5.262391672463365372E-17, 0.001077686929059507720, 0.002155373858118960796, 0.004310747716237871285 ),
 .UNSPECIFIED. ) ;
#14336 = APPLICATION_PROTOCOL_DEFINITION ( 'draft international standard', 'automotive_design', 1998, #11879 ) ;
#14337 = DIRECTION ( 'NONE',  ( 0.000000000000000000, 0.000000000000000000, -1.000000000000000000 ) ) ;
#14338 = PLANE ( 'NONE',  #9163 ) ;
#14339 = CARTESIAN_POINT ( 'NONE',  ( -9.166452524254948386, 2.202000163336201410, -48.23896987259320923 ) ) ;
#14341 = CYLINDRICAL_SURFACE ( 'NONE', #1055, 0.5000000000000004441 ) ;
#14340 = APPLICATION_CONTEXT ( 'automotive_design' ) ;
#14342 = ADVANCED_FACE ( 'NONE', ( #1316 ), #8335, .F. ) ;
#14343 = AXIS2_PLACEMENT_3D ( 'NONE', #13681, #13839, #3140 ) ;
#14344 = FACE_BOUND ( 'NONE', #11914, .T. ) ;
#14345 = DIRECTION ( 'NONE',  ( -1.000000000000000000, 0.000000000000000000, 0.000000000000000000 ) ) ;
#14346 = VECTOR ( 'NONE', #6093, 1000.000000000000000 ) ;
#14347 = CARTESIAN_POINT ( 'NONE',  ( 33.33600117268625951, -54.92996021470965928, 2.012507329417090318 ) ) ;
#14348 = PLANE ( 'NONE',  #6623 ) ;
#14349 = CARTESIAN_POINT ( 'NONE',  ( -2.688903428702175252E-15, 23.25070940071368142, 33.00000000000012790 ) ) ;
#14350 = ORIENTED_EDGE ( 'NONE', *, *, #1738, .F. ) ;
#14351 = DIRECTION ( 'NONE',  ( -1.000000000000000000, 0.000000000000000000, 0.000000000000000000 ) ) ;
#14352 = LINE ( 'NONE', #3796, #9656 ) ;
#14353 = ADVANCED_FACE ( 'NONE', ( #8178 ), #15043, .T. ) ;
#14354 = EDGE_LOOP ( 'NONE', ( #1215, #5913, #1541, #1899 ) ) ;
#14355 = VECTOR ( 'NONE', #9050, 1000.000000000000000 ) ;
#14356 = FACE_OUTER_BOUND ( 'NONE', #7474, .T. ) ;
#14357 = VECTOR ( 'NONE', #9303, 1000.000000000000000 ) ;
#14358 = CARTESIAN_POINT ( 'NONE',  ( 69.32560489365786793, -4.047139788659277926, 77.19766409531744955 ) ) ;
#14359 = DIRECTION ( 'NONE',  ( -9.251858538542971581E-17, -1.000000000000000000, 0.000000000000000000 ) ) ;
#14360 = ADVANCED_FACE ( 'NONE', ( #3553 ), #9481, .F. ) ;
#14361 = EDGE_CURVE ( 'NONE', #3181, #3011, #15103, .T. ) ;
#14362 = CARTESIAN_POINT ( 'NONE',  ( -21.58505662828840244, 4.908031226326156293, -58.00000000000012079 ) ) ;
#14363 = DIRECTION ( 'NONE',  ( 0.000000000000000000, 1.000000000000000000, 0.000000000000000000 ) ) ;
#14364 = CARTESIAN_POINT ( 'NONE',  ( 29.93026052250974445, -53.28555914634976176, 4.056187502120626398 ) ) ;
#14365 = ORIENTED_EDGE ( 'NONE', *, *, #5054, .T. ) ;
#14366 = CARTESIAN_POINT ( 'NONE',  ( -25.99999999999998934, -2.249290599286303927, -38.50000000000012790 ) ) ;
#14367 = ORIENTED_EDGE ( 'NONE', *, *, #207, .T. ) ;
#14368 = CARTESIAN_POINT ( 'NONE',  ( 52.46774229227035136, -1.764205727211077379, 60.61639468829817190 ) ) ;
#14369 = ORIENTED_EDGE ( 'NONE', *, *, #8145, .F. ) ;
#14370 = EDGE_LOOP ( 'NONE', ( #13208, #3442, #4904, #4061 ) ) ;
#14371 = CARTESIAN_POINT ( 'NONE',  ( 65.21119105374334879, -11.89996587754543711, 75.53257027772512799 ) ) ;
#14372 = DIRECTION ( 'NONE',  ( 1.000000000000000000, 0.000000000000000000, 0.000000000000000000 ) ) ;
#14373 = EDGE_CURVE ( 'NONE', #14748, #3495, #13864, .T. ) ;
#14374 = ADVANCED_FACE ( 'NONE', ( #4632 ), #14174, .T. ) ;
#14375 = CYLINDRICAL_SURFACE ( 'NONE', #13579, 4.000000000000003553 ) ;
#14376 = VERTEX_POINT ( 'NONE', #2476 ) ;
#14377 = CARTESIAN_POINT ( 'NONE',  ( 8.199792978590135561, -57.47994873761391688, 2.501453769636591495 ) ) ;
#14378 = CARTESIAN_POINT ( 'NONE',  ( -24.12883632398703782, 3.619414784477793301, 48.08465436988272756 ) ) ;
#14379 = CARTESIAN_POINT ( 'NONE',  ( 64.90552635791956959, 22.43695620243006772, 33.00000000000014211 ) ) ;
#14380 = ORIENTED_EDGE ( 'NONE', *, *, #13143, .T. ) ;
#14381 = ORIENTED_EDGE ( 'NONE', *, *, #10744, .T. ) ;
#14382 = DIRECTION ( 'NONE',  ( -1.000000000000000000, 0.000000000000000000, 0.000000000000000000 ) ) ;
#14383 = ORIENTED_EDGE ( 'NONE', *, *, #11036, .F. ) ;
#14384 = CARTESIAN_POINT ( 'NONE',  ( -22.94555154978778688, 4.515786682032536525, 48.04486892757390848 ) ) ;
#14385 = ORIENTED_EDGE ( 'NONE', *, *, #5771, .F. ) ;
#14386 = CARTESIAN_POINT ( 'NONE',  ( 30.71459926079626612, -62.29356353673582447, 3.270869388460270866 ) ) ;
#14387 = ORIENTED_EDGE ( 'NONE', *, *, #2478, .T. ) ;
#14388 = ADVANCED_BREP_SHAPE_REPRESENTATION ( '', ( #9491, #6315 ), #10740 ) ;
#14389 = DIRECTION ( 'NONE',  ( -1.000000000000000000, -1.823797295821256855E-31, 1.051347561198064835E-16 ) ) ;
#14390 = FACE_OUTER_BOUND ( 'NONE', #9989, .T. ) ;
#14391 = ORIENTED_EDGE ( 'NONE', *, *, #15200, .T. ) ;
#14392 = CARTESIAN_POINT ( 'NONE',  ( 29.10765984106734550, -64.50532980541194661, -3.862852061920468039 ) ) ;
#14393 = DIRECTION ( 'NONE',  ( 0.000000000000000000, 0.000000000000000000, 1.000000000000000000 ) ) ;
#14394 = EDGE_LOOP ( 'NONE', ( #8785, #6375, #946, #11833, #710, #14818, #1221, #12272, #1959 ) ) ;
#14395 = DIRECTION ( 'NONE',  ( 1.000000000000000000, 0.000000000000000000, 0.000000000000000000 ) ) ;
#14396 = CARTESIAN_POINT ( 'NONE',  ( 56.59738969056744651, 21.75070940071329417, -33.00000000000012790 ) ) ;
#14397 = CARTESIAN_POINT ( 'NONE',  ( -65.00000000000001421, -85.24929059928629727, -19.99999999999999645 ) ) ;
#14398 = ORIENTED_EDGE ( 'NONE', *, *, #7737, .T. ) ;
#14399 = CARTESIAN_POINT ( 'NONE',  ( -22.44582411025819368, 4.950411932228481859, 48.32458034485718912 ) ) ;
#14400 = EDGE_CURVE ( 'NONE', #11798, #11128, #11628, .T. ) ;
#14401 = ADVANCED_FACE ( 'NONE', ( #4707 ), #12101, .T. ) ;
#14402 = ORIENTED_EDGE ( 'NONE', *, *, #12291, .T. ) ;
#14403 = CARTESIAN_POINT ( 'NONE',  ( 12.36791015745245836, -56.52532528994181860, 2.500000000000000000 ) ) ;
#14404 = ADVANCED_FACE ( 'NONE', ( #12880 ), #7168, .T. ) ;
#14405 = VERTEX_POINT ( 'NONE', #3996 ) ;
#14406 = APPLICATION_PROTOCOL_DEFINITION ( 'draft international standard', 'automotive_design', 1998, #12966 ) ;
#14407 = LINE ( 'NONE', #1555, #8550 ) ;
#14408 = LINE ( 'NONE', #8622, #8434 ) ;
#14409 = DIRECTION ( 'NONE',  ( 0.4848096202550659650, 0.8746197071345572782, -0.000000000000000000 ) ) ;
#14410 = AXIS2_PLACEMENT_3D ( 'NONE', #6947, #14025, #13871 ) ;
#14411 = PLANE ( 'NONE',  #9808 ) ;
#14412 = CARTESIAN_POINT ( 'NONE',  ( -30.00000000000000000, -72.24929059928631148, -32.99999999999982236 ) ) ;
#14413 = PLANE ( 'NONE',  #2157 ) ;
#14414 = DIRECTION ( 'NONE',  ( -0.4848096202550659650, -0.8746197071345572782, 0.000000000000000000 ) ) ;
#14415 = EDGE_CURVE ( 'NONE', #4620, #14067, #3779, .T. ) ;
#14416 = CARTESIAN_POINT ( 'NONE',  ( 58.00000000000000711, 7.750709400713694741, 38.00000000000012079 ) ) ;
#14417 = CARTESIAN_POINT ( 'NONE',  ( 32.59950272815257222, -53.72645478541647890, -3.103403305059523554 ) ) ;
#14418 = ADVANCED_FACE ( 'NONE', ( #9792 ), #5160, .F. ) ;
#14419 = AXIS2_PLACEMENT_3D ( 'NONE', #6026, #2558, #6101 ) ;
#14420 = LINE ( 'NONE', #13334, #8828 ) ;
#14421 = VERTEX_POINT ( 'NONE', #4936 ) ;
#14422 = LINE ( 'NONE', #12025, #12087 ) ;
#14423 = CARTESIAN_POINT ( 'NONE',  ( 33.25875691633304143, -58.62940108252828963, -2.501915095519685384 ) ) ;
#14424 = CYLINDRICAL_SURFACE ( 'NONE', #646, 0.5000000000000001110 ) ;
#14425 = PLANE ( 'NONE',  #1644 ) ;
#14426 = CARTESIAN_POINT ( 'NONE',  ( 80.00000000000001421, -74.24929059928631148, -8.000000000000001776 ) ) ;
#14427 = CIRCLE ( 'NONE', #13925, 0.4999999999999994449 ) ;
#14428 = AXIS2_PLACEMENT_3D ( 'NONE', #7660, #11187, #1729 ) ;
#14429 = PLANE ( 'NONE',  #275 ) ;
#14430 = CARTESIAN_POINT ( 'NONE',  ( 58.00000000000000711, -2.249290599286311032, 139.1143251403882459 ) ) ;
#14431 = CIRCLE ( 'NONE', #5586, 3.000000000000002665 ) ;
#14432 = AXIS2_PLACEMENT_3D ( 'NONE', #1165, #12883, #8260 ) ;
#14433 = ORIENTED_EDGE ( 'NONE', *, *, #4577, .T. ) ;
#14434 = LINE ( 'NONE', #11035, #6151 ) ;
#14435 = UNCERTAINTY_MEASURE_WITH_UNIT (LENGTH_MEASURE( 1.000000000000000082E-05 ), #2945, 'distance_accuracy_value', 'NONE');
#14436 = EDGE_CURVE ( 'NONE', #4285, #12694, #8694, .T. ) ;
#14437 = EDGE_LOOP ( 'NONE', ( #6211, #10156, #3842, #4843 ) ) ;
#14438 = CARTESIAN_POINT ( 'NONE',  ( -25.40901433244242114, -6.686340856221296036, 48.00000000000012079 ) ) ;
#14439 = CARTESIAN_POINT ( 'NONE',  ( -2.688903428702175252E-15, 23.25070940071368142, -33.00000000000012790 ) ) ;
#14440 = ORIENTED_EDGE ( 'NONE', *, *, #449, .F. ) ;
#14441 = AXIS2_PLACEMENT_3D ( 'NONE', #8863, #8711, #12114 ) ;
#14442 = VERTEX_POINT ( 'NONE', #3701 ) ;
#14443 = CARTESIAN_POINT ( 'NONE',  ( -10.97058782713534164, -9.028420861780718454, 48.26891069786831423 ) ) ;
#14444 = CYLINDRICAL_SURFACE ( 'NONE', #1147, 8.924024642120684803 ) ;
#14445 = DIRECTION ( 'NONE',  ( 1.224646799147353207E-16, -1.000000000000000000, 0.000000000000000000 ) ) ;
#14446 = PRODUCT_DEFINITION_FORMATION_WITH_SPECIFIED_SOURCE ( 'ANY', '', #7821, .NOT_KNOWN. ) ;
#14447 = ORIENTED_EDGE ( 'NONE', *, *, #6244, .F. ) ;
#14448 = CARTESIAN_POINT ( 'NONE',  ( 8.256272429926839962, -55.33425260370182031, 2.693485533444373026 ) ) ;
#14449 = AXIS2_PLACEMENT_3D ( 'NONE', #10551, #6929, #1231 ) ;
#14450 = AXIS2_PLACEMENT_3D ( 'NONE', #15104, #13789, #3247 ) ;
#14451 = CARTESIAN_POINT ( 'NONE',  ( -12.14523415828296571, -9.827631355817223024, 57.50000000000012079 ) ) ;
#14452 = LINE ( 'NONE', #8811, #12227 ) ;
#14453 = VERTEX_POINT ( 'NONE', #10787 ) ;
#14454 = VERTEX_POINT ( 'NONE', #248 ) ;
#14455 = FACE_OUTER_BOUND ( 'NONE', #2883, .T. ) ;
#14456 = ADVANCED_FACE ( 'NONE', ( #1392 ), #8407, .T. ) ;
#14457 = ORIENTED_EDGE ( 'NONE', *, *, #13179, .F. ) ;
#14458 = CARTESIAN_POINT ( 'NONE',  ( 95.31453344691183815, 21.75070940071356418, 33.00000000000012790 ) ) ;
#14459 = VECTOR ( 'NONE', #13531, 1000.000000000000000 ) ;
#14460 = ORIENTED_EDGE ( 'NONE', *, *, #14866, .T. ) ;
#14461 = CARTESIAN_POINT ( 'NONE',  ( 29.24098086411990849, -64.27177309650618042, 3.135762038895159698 ) ) ;
#14462 = ORIENTED_EDGE ( 'NONE', *, *, #6884, .F. ) ;
#14463 = TOROIDAL_SURFACE ( 'NONE', #11753, 8.500000000000000000, 0.5000000000000000000 ) ;
#14464 = LINE ( 'NONE', #8471, #10493 ) ;
#14465 = DIRECTION ( 'NONE',  ( -0.000000000000000000, 0.000000000000000000, 1.000000000000000000 ) ) ;
#14466 = EDGE_LOOP ( 'NONE', ( #7685, #10848, #1683, #13801 ) ) ;
#14467 = CARTESIAN_POINT ( 'NONE',  ( 62.67308791069655882, 25.52935533987996664, -33.00000000000013500 ) ) ;
#14468 = ORIENTED_EDGE ( 'NONE', *, *, #9886, .F. ) ;
#14469 = DIRECTION ( 'NONE',  ( -0.8656763553492754504, -0.5006040828730772274, -1.896095000761754519E-14 ) ) ;
#14470 = PLANE ( 'NONE',  #13788 ) ;
#14471 = CARTESIAN_POINT ( 'NONE',  ( -65.00000000000001421, -85.24929059928629727, -22.49999999999999289 ) ) ;
#14472 = EDGE_LOOP ( 'NONE', ( #4996, #7673, #4534, #9498 ) ) ;
#14473 = ADVANCED_FACE ( 'NONE', ( #14331 ), #9644, .T. ) ;
#14474 = CARTESIAN_POINT ( 'NONE',  ( 66.38598137497019991, -11.47113225237460910, 72.19766410831374515 ) ) ;
#14475 = ORIENTED_EDGE ( 'NONE', *, *, #2546, .F. ) ;
#14476 = ORIENTED_EDGE ( 'NONE', *, *, #4717, .F. ) ;
#14477 = CARTESIAN_POINT ( 'NONE',  ( 67.21328690825529861, 29.52935533987996664, -21.00807340887166674 ) ) ;
#14478 = ORIENTED_EDGE ( 'NONE', *, *, #9149, .F. ) ;
#14479 = SHAPE_DEFINITION_REPRESENTATION ( #14813, #3114 ) ;
#14480 = CARTESIAN_POINT ( 'NONE',  ( 88.00000000000000000, 23.25070940071369208, -33.00000000000012790 ) ) ;
#14481 = CARTESIAN_POINT ( 'NONE',  ( -65.00000000000001421, -87.24929059928631148, 19.99999999999999645 ) ) ;
#14482 = CARTESIAN_POINT ( 'NONE',  ( -33.07225206673494711, -1.856991049495498425, 48.50000000000012079 ) ) ;
#14483 = EDGE_CURVE ( 'NONE', #10222, #8652, #12388, .T. ) ;
#14484 = CARTESIAN_POINT ( 'NONE',  ( 12.65170711616557142, -50.97709764761836482, 4.214141842892688672 ) ) ;
#14485 = DIRECTION ( 'NONE',  ( 1.000000000000000000, 0.000000000000000000, 0.000000000000000000 ) ) ;
#14486 = DIRECTION ( 'NONE',  ( -9.912705577010325549E-17, 1.000000000000000000, 1.734723475976817547E-15 ) ) ;
#14487 = CARTESIAN_POINT ( 'NONE',  ( 32.96955190781037004, -54.21180406361326476, -2.945963350965641769 ) ) ;
#14488 = AXIS2_PLACEMENT_3D ( 'NONE', #687, #9004, #1995 ) ;
#14489 = VECTOR ( 'NONE', #11543, 1000.000000000000000 ) ;
#14490 = CARTESIAN_POINT ( 'NONE',  ( -80.00000000000001421, -74.24929059928631148, -32.00000000000000000 ) ) ;
#14491 = VERTEX_POINT ( 'NONE', #12239 ) ;
#14492 = LINE ( 'NONE', #7559, #1999 ) ;
#14493 = CARTESIAN_POINT ( 'NONE',  ( -12.09280073291247426, 0.000000000000000000, -11.78977872328358067 ) ) ;
#14494 = DIRECTION ( 'NONE',  ( 0.8656763553493062036, 0.5006040828730242698, 0.000000000000000000 ) ) ;
#14495 = DIRECTION ( 'NONE',  ( 0.8746197071345572782, -0.4848096202550659650, 0.000000000000000000 ) ) ;
#14496 = EDGE_CURVE ( 'NONE', #4156, #10163, #7430, .T. ) ;
#14497 = EDGE_CURVE ( 'NONE', #13455, #3217, #9865, .T. ) ;
#14498 = PLANE ( 'NONE',  #3593 ) ;
#14499 = EDGE_CURVE ( 'NONE', #11665, #9348, #14555, .T. ) ;
#14500 = CARTESIAN_POINT ( 'NONE',  ( 64.17080745393407426, -11.91156998299096337, 72.67649750183591095 ) ) ;
#14501 = CARTESIAN_POINT ( 'NONE',  ( 27.67348840388350339, -69.39711819508848123, -4.211076768700163342 ) ) ;
#14502 = EDGE_CURVE ( 'NONE', #6181, #1998, #13094, .T. ) ;
#14503 = CARTESIAN_POINT ( 'NONE',  ( -24.54316049702162772, -7.158540003846257882, -48.36906329404664007 ) ) ;
#14504 = ORIENTED_EDGE ( 'NONE', *, *, #9296, .F. ) ;
#14505 = ORIENTED_EDGE ( 'NONE', *, *, #7226, .T. ) ;
#14506 = DIRECTION ( 'NONE',  ( -0.000000000000000000, 1.000000000000000000, -0.000000000000000000 ) ) ;
#14507 = DIRECTION ( 'NONE',  ( 0.000000000000000000, 0.000000000000000000, -1.000000000000000000 ) ) ;
#14508 = CIRCLE ( 'NONE', #10081, 9.000000000000001776 ) ;
#14509 = ORIENTED_EDGE ( 'NONE', *, *, #9276, .F. ) ;
#14510 = DIRECTION ( 'NONE',  ( 0.000000000000000000, 0.000000000000000000, -1.000000000000000000 ) ) ;
#14511 = CARTESIAN_POINT ( 'NONE',  ( 58.00000000000000711, -2.249290599286309256, 47.51982618741348574 ) ) ;
#14512 = DIRECTION ( 'NONE',  ( 0.6198786537240922323, -0.7846976836063727090, 0.000000000000000000 ) ) ;
#14513 = VERTEX_POINT ( 'NONE', #3844 ) ;
#14514 = CARTESIAN_POINT ( 'NONE',  ( 53.81626139532630759, -82.24929059928629727, 11.78977872328355048 ) ) ;
#14515 = ADVANCED_FACE ( 'NONE', ( #14251 ), #7241, .F. ) ;
#14516 = DIRECTION ( 'NONE',  ( -1.000000000000000000, -0.000000000000000000, -0.000000000000000000 ) ) ;
#14517 = DIRECTION ( 'NONE',  ( 0.000000000000000000, 0.000000000000000000, 1.000000000000000000 ) ) ;
#14518 = ORIENTED_EDGE ( 'NONE', *, *, #14178, .T. ) ;
#14519 = ORIENTED_EDGE ( 'NONE', *, *, #11196, .T. ) ;
#14520 = DIRECTION ( 'NONE',  ( 0.000000000000000000, -0.000000000000000000, 1.000000000000000000 ) ) ;
#14521 = ORIENTED_EDGE ( 'NONE', *, *, #10069, .T. ) ;
#14522 = ORIENTED_EDGE ( 'NONE', *, *, #11531, .F. ) ;
#14523 = CARTESIAN_POINT ( 'NONE',  ( 62.70356846721307420, -0.3817325368051065482, 62.84860122826521689 ) ) ;
#14524 = ORIENTED_EDGE ( 'NONE', *, *, #2357, .T. ) ;
#14525 = CARTESIAN_POINT ( 'NONE',  ( 28.59185145675465733, -64.18054652438925700, 4.118450070758925996 ) ) ;
#14526 = CIRCLE ( 'NONE', #7889, 0.4999999999999997224 ) ;
#14527 = ORIENTED_EDGE ( 'NONE', *, *, #6175, .F. ) ;
#14528 = CARTESIAN_POINT ( 'NONE',  ( 8.821484763567294607, -57.33450387999030795, -2.749014434309871469 ) ) ;
#14529 = DIRECTION ( 'NONE',  ( 0.000000000000000000, -0.000000000000000000, 1.000000000000000000 ) ) ;
#14530 = ORIENTED_EDGE ( 'NONE', *, *, #14215, .F. ) ;
#14531 = DIRECTION ( 'NONE',  ( 1.000000000000000000, 0.000000000000000000, 0.000000000000000000 ) ) ;
#14532 = CIRCLE ( 'NONE', #9876, 3.000000000000000888 ) ;
#14533 = ORIENTED_EDGE ( 'NONE', *, *, #122, .T. ) ;
#14534 = EDGE_CURVE ( 'NONE', #2944, #5593, #2700, .T. ) ;
#14535 = ADVANCED_FACE ( 'NONE', ( #390 ), #5086, .T. ) ;
#14536 = AXIS2_PLACEMENT_3D ( 'NONE', #11262, #7816, #13808 ) ;
#14537 = DIRECTION ( 'NONE',  ( -0.000000000000000000, -0.000000000000000000, 1.000000000000000000 ) ) ;
#14538 = DIRECTION ( 'NONE',  ( -0.000000000000000000, -0.000000000000000000, -1.000000000000000000 ) ) ;
#14539 = ORIENTED_EDGE ( 'NONE', *, *, #15114, .F. ) ;
#14540 = MANIFOLD_SOLID_BREP ( 'Fillet5', #11932 ) ;
#14541 = CARTESIAN_POINT ( 'NONE',  ( 73.69809405469877106, 29.52935533987996664, -21.00807340887166674 ) ) ;
#14542 = ORIENTED_EDGE ( 'NONE', *, *, #11411, .T. ) ;
#14543 =( GEOMETRIC_REPRESENTATION_CONTEXT ( 3 ) GLOBAL_UNCERTAINTY_ASSIGNED_CONTEXT ( ( #13056 ) ) GLOBAL_UNIT_ASSIGNED_CONTEXT ( ( #10177, #4309, #2006 ) ) REPRESENTATION_CONTEXT ( 'NONE', 'WORKASPACE' ) );
#14544 = EDGE_LOOP ( 'NONE', ( #5287, #672, #2457, #3990 ) ) ;
#14545 = CIRCLE ( 'NONE', #1273, 9.000000000000001776 ) ;
#14546 = DIRECTION ( 'NONE',  ( -0.000000000000000000, -0.000000000000000000, -1.000000000000000000 ) ) ;
#14547 = APPLICATION_PROTOCOL_DEFINITION ( 'draft international standard', 'automotive_design', 1998, #9533 ) ;
#14548 = DIRECTION ( 'NONE',  ( -1.000000000000000000, 0.000000000000000000, 0.000000000000000000 ) ) ;
#14549 = DIRECTION ( 'NONE',  ( 0.000000000000000000, 0.000000000000000000, 1.000000000000000000 ) ) ;
#14550 = ADVANCED_FACE ( 'NONE', ( #2926 ), #8994, .T. ) ;
#14551 = CARTESIAN_POINT ( 'NONE',  ( -11.86108202630535224, -9.639858853941328576, -48.38337049880509255 ) ) ;
#14552 = ORIENTED_EDGE ( 'NONE', *, *, #5136, .T. ) ;
#14553 = EDGE_CURVE ( 'NONE', #10521, #3380, #10386, .T. ) ;
#14554 = CARTESIAN_POINT ( 'NONE',  ( 9.841858720825518603, -62.60511169126380082, 2.715102820267620398 ) ) ;
#14555 = CIRCLE ( 'NONE', #2523, 4.505436745857433145 ) ;
#14556 = CARTESIAN_POINT ( 'NONE',  ( 57.26556849154462725, -7.256479411572841265, 48.51982618741349285 ) ) ;
#14557 = CIRCLE ( 'NONE', #5220, 1.000000000000007550 ) ;
#14558 = CARTESIAN_POINT ( 'NONE',  ( 65.00000000000001421, -85.24929059928629727, -22.49999999999999289 ) ) ;
#14559 = CARTESIAN_POINT ( 'NONE',  ( 25.81270058232203013, 23.25070940071368852, 139.1143251403882459 ) ) ;
#14560 = AXIS2_PLACEMENT_3D ( 'NONE', #4674, #9297, #1122 ) ;
#14561 = CARTESIAN_POINT ( 'NONE',  ( -9.456839514482959785, 2.659958822950722279, 48.50000000000011369 ) ) ;
#14562 = ORIENTED_EDGE ( 'NONE', *, *, #5087, .F. ) ;
#14563 = SURFACE_STYLE_USAGE ( .BOTH. , #4012 ) ;
#14564 = CARTESIAN_POINT ( 'NONE',  ( 32.90197589884652274, -57.33450387999030085, -2.749014434309875909 ) ) ;
#14565 = AXIS2_PLACEMENT_3D ( 'NONE', #10276, #14966, #12655 ) ;
#14566 = SHAPE_REPRESENTATION_RELATIONSHIP ( 'NONE' , 'NONE' ,  #10411, #13442 ) ;
#14567 = CARTESIAN_POINT ( 'NONE',  ( 33.52235686305655804, -57.48563641131178770, -1.816685854991392457 ) ) ;
#14568 = EDGE_CURVE ( 'NONE', #7720, #246, #5385, .T. ) ;
#14569 = CARTESIAN_POINT ( 'NONE',  ( 21.74884261173415467, -85.24929059928631148, -6.000000000000000888 ) ) ;
#14570 = CIRCLE ( 'NONE', #5736, 1.000000000000001554 ) ;
#14571 = EDGE_CURVE ( 'NONE', #612, #6145, #15054, .T. ) ;
#14572 = LINE ( 'NONE', #11107, #990 ) ;
#14573 = CARTESIAN_POINT ( 'NONE',  ( 28.56964104117922076, -65.59433601606471598, -3.409308316089457502 ) ) ;
#14574 = EDGE_LOOP ( 'NONE', ( #5244, #360, #14611, #11692, #8263, #5051, #10275, #14519, #2259, #4983, #8814, #1391, #2904, #4453, #7950, #1047, #7604, #2488, #4609, #3466, #11405, #809, #2328, #2556, #826, #10064, #12430, #13601, #584, #14803, #7764, #8318, #10389, #4191, #3700, #9240, #9717, #14530, #11481, #8673, #13701, #794, #13155, #12765, #529, #729, #3558, #13041, #11561, #7536, #8722, #5193, #14892, #5826, #2680, #12845, #6314, #12754, #11261, #9983, #8018, #10903, #12468, #12308, #589, #14365 ) ) ;
#14575 = VECTOR ( 'NONE', #11680, 1000.000000000000000 ) ;
#14576 = LINE ( 'NONE', #1581, #2464 ) ;
#14577 = VECTOR ( 'NONE', #8913, 1000.000000000000000 ) ;
#14578 = ORIENTED_EDGE ( 'NONE', *, *, #1040, .T. ) ;
#14579 = CARTESIAN_POINT ( 'NONE',  ( 20.86173033120691045, -52.24929059928630437, 6.000000000000000000 ) ) ;
#14580 = EDGE_LOOP ( 'NONE', ( #2990, #8148, #12910, #761 ) ) ;
#14581 = LINE ( 'NONE', #6499, #9892 ) ;
#14582 = DIRECTION ( 'NONE',  ( -1.000000000000000000, 0.000000000000000000, 0.000000000000000000 ) ) ;
#14583 = EDGE_CURVE ( 'NONE', #11220, #14995, #8841, .T. ) ;
#14584 = DIRECTION ( 'NONE',  ( 1.000000000000000000, 0.000000000000000000, 0.000000000000000000 ) ) ;
#14585 = CARTESIAN_POINT ( 'NONE',  ( 11.55440981570039938, -53.31390540393576316, 3.970772651015708199 ) ) ;
#14586 = AXIS2_PLACEMENT_3D ( 'NONE', #152, #10545, #14237 ) ;
#14587 = DIRECTION ( 'NONE',  ( 0.8746197071345572782, -0.4848096202550659650, 0.000000000000000000 ) ) ;
#14588 = DIRECTION ( 'NONE',  ( 0.000000000000000000, 1.734723475976817547E-15, -1.000000000000000000 ) ) ;
#14589 = ADVANCED_FACE ( 'NONE', ( #13535 ), #14613, .T. ) ;
#14590 = ORIENTED_EDGE ( 'NONE', *, *, #4616, .F. ) ;
#14591 = EDGE_CURVE ( 'NONE', #11933, #3181, #8922, .T. ) ;
#14592 = CARTESIAN_POINT ( 'NONE',  ( -21.16581936427349575, -2.249290599286303483, 50.50000000000012079 ) ) ;
#14593 = EDGE_LOOP ( 'NONE', ( #4550, #14381, #2822, #6956 ) ) ;
#14594 = CARTESIAN_POINT ( 'NONE',  ( 30.17008156804327612, -53.31401535610196163, -3.970404413101018104 ) ) ;
#14595 = ORIENTED_EDGE ( 'NONE', *, *, #13486, .F. ) ;
#14596 = CARTESIAN_POINT ( 'NONE',  ( 27.85548922659574700, -68.67521603617417725, 4.260811380381850810 ) ) ;
#14597 = CARTESIAN_POINT ( 'NONE',  ( 69.40535631463106370, -3.419795260923345293, 71.40614770598537575 ) ) ;
#14598 = ORIENTED_EDGE ( 'NONE', *, *, #13676, .F. ) ;
#14599 = DIRECTION ( 'NONE',  ( -0.000000000000000000, 1.445602896647339163E-16, 1.000000000000000000 ) ) ;
#14600 = CARTESIAN_POINT ( 'NONE',  ( -9.271822474830662131, -6.861803161813125662, 47.50000000000012079 ) ) ;
#14601 = EDGE_LOOP ( 'NONE', ( #1979, #6353, #13665, #9605, #9487, #3475, #2387, #10192, #375, #10359 ) ) ;
#14602 = CARTESIAN_POINT ( 'NONE',  ( 30.71459926079771918, -62.29356353674184987, -3.270869388464555438 ) ) ;
#14603 = ORIENTED_EDGE ( 'NONE', *, *, #13408, .T. ) ;
#14604 = DIRECTION ( 'NONE',  ( -0.000000000000000000, 0.000000000000000000, -1.000000000000000000 ) ) ;
#14605 = DIRECTION ( 'NONE',  ( -0.000000000000000000, 0.000000000000000000, 1.000000000000000000 ) ) ;
#14606 = DIRECTION ( 'NONE',  ( -0.5394184268574523378, 0.8420378618367652113, 0.000000000000000000 ) ) ;
#14607 = VERTEX_POINT ( 'NONE', #1051 ) ;
#14608 = CARTESIAN_POINT ( 'NONE',  ( 67.21328690825531282, 22.43695620243006772, 84.20452624982236500 ) ) ;
#14609 = ORIENTED_EDGE ( 'NONE', *, *, #15218, .T. ) ;
#14610 = ORIENTED_EDGE ( 'NONE', *, *, #6974, .F. ) ;
#14611 = ORIENTED_EDGE ( 'NONE', *, *, #1382, .T. ) ;
#14612 = EDGE_CURVE ( 'NONE', #3738, #791, #9292, .T. ) ;
#14613 = SPHERICAL_SURFACE ( 'NONE', #5730, 1.000000000000000000 ) ;
#14614 = APPLICATION_PROTOCOL_DEFINITION ( 'draft international standard', 'automotive_design', 1998, #3220 ) ;
#14615 = CYLINDRICAL_SURFACE ( 'NONE', #1898, 4.000000000000003553 ) ;
#14616 = DIRECTION ( 'NONE',  ( 0.000000000000000000, 1.000000000000000000, 0.000000000000000000 ) ) ;
#14617 =( BOUNDED_SURFACE ( )  B_SPLINE_SURFACE ( 3, 2, ( 
 ( #840, #8851, #8931 ),
 ( #8007, #14701, #14850 ),
 ( #13622, #12470, #4300 ),
 ( #5549, #918, #4153 ),
 ( #10399, #15094, #4543 ),
 ( #9245, #13933, #5711 ),
 ( #10880, #1405, #10801 ),
 ( #10652, #113, #14191 ),
 ( #7332, #3934, #8347 ),
 ( #4798, #3713, #3860 ),
 ( #338, #14487, #1333 ),
 ( #14265, #5030, #3793 ),
 ( #12020, #14417, #8631 ),
 ( #8562, #11944, #12105 ),
 ( #9581, #2414, #1565 ),
 ( #9497, #9735, #6114 ),
 ( #7108, #261, #10954 ),
 ( #2639, #1486, #6191 ),
 ( #13260, #8498, #11795 ),
 ( #2714, #1251, #13183 ),
 ( #5965, #8422, #10721 ),
 ( #6264, #6037, #3646 ),
 ( #13115, #2570, #7408 ),
 ( #13038, #4948, #2486 ) ),
 .UNSPECIFIED., .F., .F., .T. ) 
 B_SPLINE_SURFACE_WITH_KNOTS ( ( 4, 2, 2, 2, 2, 2, 2, 2, 2, 2, 2, 4 ),
 ( 3, 3 ),
 ( 0.000000000000000000, 0.0007560557787111729612, 0.001512111557422345922, 0.001890139446777932240, 0.002268167336133518775, 0.003024223114844691845, 0.003402251004200278379, 0.003780278893555864481, 0.004158306782911451449, 0.004536334672267037550, 0.005292390450978210620, 0.006048446229689383689 ),
 ( 0.000000000000000000, 1.000000000000000000 ),
 .UNSPECIFIED. ) 
 GEOMETRIC_REPRESENTATION_ITEM ( )  RATIONAL_B_SPLINE_SURFACE ( (
 ( 1.000000000000000000, 0.8250833044923658877, 1.000000000000000000),
 ( 1.000000000000000000, 0.8244629924933467580, 1.000000000000000000),
 ( 1.000000000000000000, 0.8228453557281663056, 1.000000000000000000),
 ( 1.000000000000000000, 0.8179470878186148042, 1.000000000000000000),
 ( 1.000000000000000000, 0.8146336382298167145, 1.000000000000000000),
 ( 1.000000000000000000, 0.8088012687532515343, 1.000000000000000000),
 ( 1.000000000000000000, 0.8067039814524846753, 1.000000000000000000),
 ( 1.000000000000000000, 0.8022097056812232951, 1.000000000000000000),
 ( 1.000000000000000000, 0.7997977307760982812, 1.000000000000000000),
 ( 1.000000000000000000, 0.7922670365021369232, 1.000000000000000000),
 ( 1.000000000000000000, 0.7868330064134674284, 1.000000000000000000),
 ( 1.000000000000000000, 0.7779933494262166738, 1.000000000000000000),
 ( 1.000000000000000000, 0.7749217965225499993, 1.000000000000000000),
 ( 1.000000000000000000, 0.7686646892562868372, 1.000000000000000000),
 ( 1.000000000000000000, 0.7654626812325054930, 1.000000000000000000),
 ( 1.000000000000000000, 0.7588889951604184114, 1.000000000000000000),
 ( 1.000000000000000000, 0.7555173610299135145, 1.000000000000000000),
 ( 1.000000000000000000, 0.7485733441930104703, 1.000000000000000000),
 ( 1.000000000000000000, 0.7449916546359187652, 1.000000000000000000),
 ( 1.000000000000000000, 0.7341394734815585021, 1.000000000000000000),
 ( 1.000000000000000000, 0.7266881283996446950, 1.000000000000000000),
 ( 1.000000000000000000, 0.7111189506802038096, 1.000000000000000000),
 ( 1.000000000000000000, 0.7029851397915697353, 1.000000000000000000),
 ( 1.000000000000000000, 0.6947298545087505772, 1.000000000000000000) ) ) 
 REPRESENTATION_ITEM ( '' )  SURFACE ( )  );
#14618 = CARTESIAN_POINT ( 'NONE',  ( -10.80198322015283097, -8.784136766666819085, -47.93908580834070676 ) ) ;
#14619 = ORIENTED_EDGE ( 'NONE', *, *, #3030, .T. ) ;
#14620 = CARTESIAN_POINT ( 'NONE',  ( 65.32988938321494743, -11.07158469721469629, 72.16329424003777149 ) ) ;
#14621 = DIRECTION ( 'NONE',  ( 0.000000000000000000, 0.000000000000000000, 1.000000000000000000 ) ) ;
#14622 = CARTESIAN_POINT ( 'NONE',  ( -25.49999999999998934, -2.249290599286304815, -38.00000000000012079 ) ) ;
#14623 = CARTESIAN_POINT ( 'NONE',  ( 14.04356807544018437, -66.53205946168881724, -4.446982897617355768 ) ) ;
#14624 = ORIENTED_EDGE ( 'NONE', *, *, #1195, .T. ) ;
#14625 = CARTESIAN_POINT ( 'NONE',  ( 14.38963276113425138, -69.39711819508849544, -4.502057496415714510 ) ) ;
#14626 = CARTESIAN_POINT ( 'NONE',  ( -9.391954890838034586, 2.559027098228045638, 47.99579695943414492 ) ) ;
#14627 = EDGE_CURVE ( 'NONE', #7613, #2221, #80, .T. ) ;
#14628 = ORIENTED_EDGE ( 'NONE', *, *, #2260, .F. ) ;
#14629 = EDGE_CURVE ( 'NONE', #304, #8543, #12755, .T. ) ;
#14630 = DIRECTION ( 'NONE',  ( 0.000000000000000000, 1.000000000000000000, -0.000000000000000000 ) ) ;
#14631 = DIRECTION ( 'NONE',  ( -0.9744556954135537019, 0.2245798247307348450, 0.000000000000000000 ) ) ;
#14632 = VECTOR ( 'NONE', #7403, 1000.000000000000000 ) ;
#14633 = CARTESIAN_POINT ( 'NONE',  ( 58.00000000000000711, -2.249290599286309256, 71.19766410831374515 ) ) ;
#14634 = ORIENTED_EDGE ( 'NONE', *, *, #11338, .T. ) ;
#14635 = FACE_OUTER_BOUND ( 'NONE', #11537, .T. ) ;
#14636 = DIRECTION ( 'NONE',  ( 0.000000000000000000, 0.000000000000000000, 1.000000000000000000 ) ) ;
#14637 = CARTESIAN_POINT ( 'NONE',  ( -24.54316048551696028, -7.158540021523408292, -57.50000000000012079 ) ) ;
#14638 = DIRECTION ( 'NONE',  ( -0.000000000000000000, 0.000000000000000000, 1.000000000000000000 ) ) ;
#14639 = DIRECTION ( 'NONE',  ( -0.000000000000000000, -0.000000000000000000, -1.000000000000000000 ) ) ;
#14640 = CIRCLE ( 'NONE', #3345, 0.7892041907098262810 ) ;
#14641 = ORIENTED_EDGE ( 'NONE', *, *, #8145, .T. ) ;
#14642 = EDGE_CURVE ( 'NONE', #9111, #355, #6948, .T. ) ;
#14643 = CARTESIAN_POINT ( 'NONE',  ( 93.56770215592470663, 0.000000000000000000, 139.1143251403882459 ) ) ;
#14644 = VERTEX_POINT ( 'NONE', #4063 ) ;
#14645 = CARTESIAN_POINT ( 'NONE',  ( -21.85476584171713199, 5.329050157244540564, 57.50000000000012079 ) ) ;
#14646 = FACE_OUTER_BOUND ( 'NONE', #506, .T. ) ;
#14647 = ORIENTED_EDGE ( 'NONE', *, *, #737, .F. ) ;
#14649 = ORIENTED_EDGE ( 'NONE', *, *, #12996, .T. ) ;
#14648 = DIRECTION ( 'NONE',  ( 0.000000000000000000, 0.000000000000000000, -1.000000000000000000 ) ) ;
#14650 = CARTESIAN_POINT ( 'NONE',  ( -1.197457146693715613, -2.220571218158943871, 48.50000000000012079 ) ) ;
#14651 = ORIENTED_EDGE ( 'NONE', *, *, #12107, .F. ) ;
#14652 = CIRCLE ( 'NONE', #2383, 9.000000000000001776 ) ;
#14653 = AXIS2_PLACEMENT_3D ( 'NONE', #13578, #14728, #13500 ) ;
#14654 = CYLINDRICAL_SURFACE ( 'NONE', #2243, 0.7892041907098262810 ) ;
#14655 = CARTESIAN_POINT ( 'NONE',  ( 10.03094031226078897, -52.93050895625587771, 3.457921359511975989 ) ) ;
#14656 = VECTOR ( 'NONE', #11052, 1000.000000000000000 ) ;
#14657 = AXIS2_PLACEMENT_3D ( 'NONE', #2401, #10565, #11707 ) ;
#14658 = DIRECTION ( 'NONE',  ( 0.000000000000000000, 0.000000000000000000, 1.000000000000000000 ) ) ;
#14659 = LINE ( 'NONE', #6581, #13454 ) ;
#14660 = ADVANCED_FACE ( 'NONE', ( #13462 ), #3523, .F. ) ;
#14661 = ORIENTED_EDGE ( 'NONE', *, *, #10450, .F. ) ;
#14662 = CIRCLE ( 'NONE', #2133, 0.7892041907098263920 ) ;
#14663 = CARTESIAN_POINT ( 'NONE',  ( 10.23047706855496664, -60.71197230342421136, 3.050751728647393080 ) ) ;
#14664 = ORIENTED_EDGE ( 'NONE', *, *, #1349, .T. ) ;
#14665 = DIRECTION ( 'NONE',  ( -1.000000000000000000, -0.000000000000000000, -0.000000000000000000 ) ) ;
#14666 = ORIENTED_EDGE ( 'NONE', *, *, #706, .F. ) ;
#14667 = DIRECTION ( 'NONE',  ( -0.000000000000000000, 1.000000000000000000, 1.445602896647339163E-16 ) ) ;
#14668 = CARTESIAN_POINT ( 'NONE',  ( 69.46098093241307936, -2.556544511925992857, 72.19317000922296756 ) ) ;
#14669 = AXIS2_PLACEMENT_3D ( 'NONE', #7920, #5535, #10220 ) ;
#14670 = DIRECTION ( 'NONE',  ( 1.000000000000000000, 1.782910239198384762E-15, 0.000000000000000000 ) ) ;
#14671 = FACE_OUTER_BOUND ( 'NONE', #13519, .T. ) ;
#14672 = ORIENTED_EDGE ( 'NONE', *, *, #12810, .T. ) ;
#14673 = AXIS2_PLACEMENT_3D ( 'NONE', #1993, #12628, #3231 ) ;
#14674 = EDGE_CURVE ( 'NONE', #14491, #14799, #790, .T. ) ;
#14675 = EDGE_CURVE ( 'NONE', #10980, #11609, #14064, .T. ) ;
#14676 = FACE_OUTER_BOUND ( 'NONE', #10694, .T. ) ;
#14677 = ORIENTED_EDGE ( 'NONE', *, *, #9616, .T. ) ;
#14678 = CARTESIAN_POINT ( 'NONE',  ( 80.00000000000001421, -74.24929059928631148, 8.000000000000001776 ) ) ;
#14679 = DIRECTION ( 'NONE',  ( -0.000000000000000000, -0.000000000000000000, -1.000000000000000000 ) ) ;
#14680 = B_SPLINE_CURVE_WITH_KNOTS ( 'NONE', 3,
 ( #2291, #12995, #3525, #13065, #13906, #15140, #2522, #10601, #4826, #7212 ),
 .UNSPECIFIED., .F., .F.,
 ( 4, 2, 2, 2, 4 ),
 ( 7.866258489732282489E-18, 0.002320432257317498782, 0.004640864514634989758, 0.006961296771952480734, 0.009281729029269972578 ),
 .UNSPECIFIED. ) ;
#14681 = DIRECTION ( 'NONE',  ( 0.000000000000000000, 0.000000000000000000, -1.000000000000000000 ) ) ;
#14682 = ADVANCED_FACE ( 'NONE', ( #10677 ), #212, .F. ) ;
#14683 = CIRCLE ( 'NONE', #12467, 4.665819364273509073 ) ;
#14684 = ORIENTED_EDGE ( 'NONE', *, *, #7910, .T. ) ;
#14685 = CARTESIAN_POINT ( 'NONE',  ( 0.000000000000000000, 21.75070940071309167, 33.00000000000012790 ) ) ;
#14686 = ORIENTED_EDGE ( 'NONE', *, *, #4364, .T. ) ;
#14687 = PRODUCT_DEFINITION_SHAPE ( 'NONE', 'NONE',  #5056 ) ;
#14688 = CIRCLE ( 'NONE', #1425, 0.7892041907098262810 ) ;
#14689 = VERTEX_POINT ( 'NONE', #1434 ) ;
#14690 = ORIENTED_EDGE ( 'NONE', *, *, #13545, .F. ) ;
#14691 = FILL_AREA_STYLE_COLOUR ( '', #9415 ) ;
#14692 = DIRECTION ( 'NONE',  ( 0.8746197071345572782, -0.4848096202550659650, 0.000000000000000000 ) ) ;
#14693 = CARTESIAN_POINT ( 'NONE',  ( 0.000000000000000000, 21.75070940071329417, 33.00000000000012790 ) ) ;
#14694 = VECTOR ( 'NONE', #12451, 1000.000000000000000 ) ;
#14695 = LINE ( 'NONE', #5391, #2839 ) ;
#14696 = EDGE_LOOP ( 'NONE', ( #14468, #13384 ) ) ;
#14697 = ORIENTED_EDGE ( 'NONE', *, *, #10557, .T. ) ;
#14698 = AXIS2_PLACEMENT_3D ( 'NONE', #1197, #12978, #14277 ) ;
#14699 = CARTESIAN_POINT ( 'NONE',  ( -8.655068852960594583, 2.300722221922764543, -48.05421924268924272 ) ) ;
#14700 = CARTESIAN_POINT ( 'NONE',  ( 60.05137561479872232, 2.911430354694811484, 60.61639468829817190 ) ) ;
#14701 = CARTESIAN_POINT ( 'NONE',  ( 33.59357299507875894, -57.17459804182058036, -2.501046471589234876 ) ) ;
#14702 = EDGE_CURVE ( 'NONE', #12099, #3816, #3977, .T. ) ;
#14703 = LINE ( 'NONE', #7709, #11127 ) ;
#14704 = CARTESIAN_POINT ( 'NONE',  ( 0.000000000000000000, 15.25070940071369563, 33.00000000000012790 ) ) ;
#14705 = VERTEX_POINT ( 'NONE', #4900 ) ;
#14706 = FACE_OUTER_BOUND ( 'NONE', #231, .T. ) ;
#14707 = DIRECTION ( 'NONE',  ( -0.000000000000000000, 0.000000000000000000, 1.000000000000000000 ) ) ;
#14708 = ORIENTED_EDGE ( 'NONE', *, *, #10748, .T. ) ;
#14709 = CARTESIAN_POINT ( 'NONE',  ( 28.81202928791190843, -63.78335865426900142, -4.036657210498111326 ) ) ;
#14710 =( BOUNDED_SURFACE ( )  B_SPLINE_SURFACE ( 3, 2, ( 
 ( #4635, #1477, #8261 ),
 ( #7245, #7018, #11864 ),
 ( #12953, #9649, #104 ),
 ( #3783, #4790, #9485 ) ),
 .UNSPECIFIED., .F., .F., .F. ) 
 B_SPLINE_SURFACE_WITH_KNOTS ( ( 4, 4 ),
 ( 3, 3 ),
 ( 0.000000000000000000, 0.001771943201165739230 ),
 ( 0.000000000000000000, 1.000000000000000000 ),
 .UNSPECIFIED. ) 
 GEOMETRIC_REPRESENTATION_ITEM ( )  RATIONAL_B_SPLINE_SURFACE ( (
 ( 1.000000000000000000, 0.8250833044923668869, 1.000000000000000000),
 ( 1.000000000000000000, 0.8269348987755763547, 1.000000000000000000),
 ( 1.000000000000000000, 0.8288551047899433977, 1.000000000000000000),
 ( 1.000000000000000000, 0.8308543624379425285, 1.000000000000000000) ) ) 
 REPRESENTATION_ITEM ( '' )  SURFACE ( )  );
#14711 = DIRECTION ( 'NONE',  ( 0.000000000000000000, 0.000000000000000000, 1.000000000000000000 ) ) ;
#14712 = ORIENTED_EDGE ( 'NONE', *, *, #10035, .F. ) ;
#14713 = VECTOR ( 'NONE', #3694, 1000.000000000000000 ) ;
#14714 = CARTESIAN_POINT ( 'NONE',  ( 33.12442989620986822, -59.21224831720011395, -1.832439066039627251 ) ) ;
#14715 = ADVANCED_FACE ( 'NONE', ( #1118 ), #9915, .F. ) ;
#14716 = ADVANCED_FACE ( 'NONE', ( #12351 ), #6282, .T. ) ;
#14717 = DIRECTION ( 'NONE',  ( 0.000000000000000000, 0.000000000000000000, -1.000000000000000000 ) ) ;
#14718 = AXIS2_PLACEMENT_3D ( 'NONE', #2093, #7724, #12409 ) ;
#14719 = AXIS2_PLACEMENT_3D ( 'NONE', #7799, #12492, #11321 ) ;
#14720 = DIRECTION ( 'NONE',  ( 1.000000000000000000, 0.000000000000000000, 0.000000000000000000 ) ) ;
#14721 = VERTEX_POINT ( 'NONE', #575 ) ;
#14722 = CARTESIAN_POINT ( 'NONE',  ( 82.49066175147797253, 23.25070940071369208, 84.20452624982236500 ) ) ;
#14723 = EDGE_LOOP ( 'NONE', ( #3693, #7048, #10564, #1256 ) ) ;
#14724 = DIRECTION ( 'NONE',  ( -1.000000000000000000, 0.000000000000000000, 0.000000000000000000 ) ) ;
#14725 = FACE_OUTER_BOUND ( 'NONE', #14211, .T. ) ;
#14726 = ORIENTED_EDGE ( 'NONE', *, *, #5966, .T. ) ;
#14727 = CARTESIAN_POINT ( 'NONE',  ( -9.871163676013017252, -8.117995983050501962, 48.08465436988272046 ) ) ;
#14728 = DIRECTION ( 'NONE',  ( -0.000000000000000000, 0.000000000000000000, 1.000000000000000000 ) ) ;
#14729 = CIRCLE ( 'NONE', #3438, 4.000000000000000000 ) ;
#14730 = AXIS2_PLACEMENT_3D ( 'NONE', #14722, #13493, #3038 ) ;
#14731 = CARTESIAN_POINT ( 'NONE',  ( 9.841896756782944067, -61.30062302791114348, 2.840369378987775306 ) ) ;
#14732 = EDGE_CURVE ( 'NONE', #10867, #13354, #1807, .T. ) ;
#14733 = CARTESIAN_POINT ( 'NONE',  ( -12.33418063572647938, -2.249290599286303927, 57.50000000000012079 ) ) ;
#14734 = CARTESIAN_POINT ( 'NONE',  ( 33.52235686305655804, -57.48563641131178770, -1.816685854991392457 ) ) ;
#14735 = CARTESIAN_POINT ( 'NONE',  ( 80.00000000000001421, -87.24929059928629727, 0.000000000000000000 ) ) ;
#14736 = LINE ( 'NONE', #11195, #14927 ) ;
#14737 = CIRCLE ( 'NONE', #9611, 5.496540510819668768 ) ;
#14738 = ORIENTED_EDGE ( 'NONE', *, *, #9756, .T. ) ;
#14739 = CARTESIAN_POINT ( 'NONE',  ( 65.00000000000001421, -85.27429059928630295, 19.99999999999999645 ) ) ;
#14740 = ORIENTED_EDGE ( 'NONE', *, *, #12360, .T. ) ;
#14741 = ORIENTED_EDGE ( 'NONE', *, *, #11378, .T. ) ;
#14742 = CARTESIAN_POINT ( 'NONE',  ( 32.06570158546600169, -54.31552982368702231, -3.256647958671372134 ) ) ;
#14743 = EDGE_LOOP ( 'NONE', ( #12649, #10922, #11006, #10577, #9040, #11512, #13731, #13093 ) ) ;
#14744 = DIRECTION ( 'NONE',  ( 1.000000000000000000, 0.000000000000000000, 0.000000000000000000 ) ) ;
#14745 = CARTESIAN_POINT ( 'NONE',  ( -25.21252699837112132, -6.998437922861947769, -57.50000000000012079 ) ) ;
#14746 = DIRECTION ( 'NONE',  ( -0.000000000000000000, 0.000000000000000000, -1.000000000000000000 ) ) ;
#14747 = DIRECTION ( 'NONE',  ( -0.000000000000000000, -0.000000000000000000, 1.000000000000000000 ) ) ;
#14748 = VERTEX_POINT ( 'NONE', #10973 ) ;
#14749 = AXIS2_PLACEMENT_3D ( 'NONE', #14794, #12262, #5266 ) ;
#14750 = CARTESIAN_POINT ( 'NONE',  ( 27.85761975137823043, -68.67486713608998627, -3.656664647162143122 ) ) ;
#14751 = ORIENTED_EDGE ( 'NONE', *, *, #12529, .T. ) ;
#14752 = CARTESIAN_POINT ( 'NONE',  ( 11.55751249766752764, -53.31348408104178560, -3.971884189131345444 ) ) ;
#14753 = DIRECTION ( 'NONE',  ( 0.000000000000000000, -1.000000000000000000, 0.000000000000000000 ) ) ;
#14754 = EDGE_CURVE ( 'NONE', #6995, #3172, #6219, .T. ) ;
#14755 = FACE_OUTER_BOUND ( 'NONE', #4040, .T. ) ;
#14756 = ORIENTED_EDGE ( 'NONE', *, *, #2725, .T. ) ;
#14757 = CARTESIAN_POINT ( 'NONE',  ( 10.00023835250150483, -61.42570632716525125, -2.132522520905374197 ) ) ;
#14758 = EDGE_CURVE ( 'NONE', #1978, #5126, #9901, .T. ) ;
#14759 = ORIENTED_EDGE ( 'NONE', *, *, #12773, .T. ) ;
#14760 = EDGE_LOOP ( 'NONE', ( #8707, #4703, #12772, #12399 ) ) ;
#14761 = ADVANCED_FACE ( 'NONE', ( #13212, #11186, #4105 ), #10907, .F. ) ;
#14762 = EDGE_LOOP ( 'NONE', ( #2682, #6917, #4057, #9845 ) ) ;
#14763 = CARTESIAN_POINT ( 'NONE',  ( 76.14589960879430919, -7.734310727912411920, 75.19766410831374515 ) ) ;
#14764 = VECTOR ( 'NONE', #1355, 1000.000000000000000 ) ;
#14765 = CONTEXT_DEPENDENT_SHAPE_REPRESENTATION ( #13240, #2733 ) ;
#14766 = LINE ( 'NONE', #11526, #14937 ) ;
#14767 = CARTESIAN_POINT ( 'NONE',  ( 88.00000000000001421, 10.75070940071369208, -33.00000000000012790 ) ) ;
#14768 = EDGE_CURVE ( 'NONE', #10906, #2535, #14581, .T. ) ;
#14769 =( GEOMETRIC_REPRESENTATION_CONTEXT ( 3 ) GLOBAL_UNCERTAINTY_ASSIGNED_CONTEXT ( ( #11663 ) ) GLOBAL_UNIT_ASSIGNED_CONTEXT ( ( #14044, #11654, #10585 ) ) REPRESENTATION_CONTEXT ( 'NONE', 'WORKASPACE' ) );
#14770 = CARTESIAN_POINT ( 'NONE',  ( -9.271822474830662131, -6.861803161813125662, -47.50000000000012079 ) ) ;
#14771 = AXIS2_PLACEMENT_3D ( 'NONE', #9995, #9856, #7469 ) ;
#14772 = ORIENTED_EDGE ( 'NONE', *, *, #6579, .F. ) ;
#14773 = DIRECTION ( 'NONE',  ( -0.000000000000000000, 0.000000000000000000, 1.000000000000000000 ) ) ;
#14774 = CARTESIAN_POINT ( 'NONE',  ( 64.48765185601422445, -11.70201852112108121, 71.95059996449334960 ) ) ;
#14775 = DIRECTION ( 'NONE',  ( 1.000000000000000000, -8.673617379884027583E-15, 0.000000000000000000 ) ) ;
#14776 = DIRECTION ( 'NONE',  ( 0.000000000000000000, -1.000000000000000000, 0.000000000000000000 ) ) ;
#14777 = CARTESIAN_POINT ( 'NONE',  ( 10.87912556055781543, -61.22098757970782401, -3.286659897583100065 ) ) ;
#14778 = EDGE_CURVE ( 'NONE', #13652, #12295, #2881, .T. ) ;
#14779 = ORIENTED_EDGE ( 'NONE', *, *, #6974, .T. ) ;
#14780 = VECTOR ( 'NONE', #12111, 1000.000000000000000 ) ;
#14781 = CARTESIAN_POINT ( 'NONE',  ( 63.43853564383336874, -3.373351419973840581, 60.61639468829817190 ) ) ;
#14782 = ADVANCED_FACE ( 'NONE', ( #9753 ), #5274, .F. ) ;
#14783 = PLANE ( 'NONE',  #6633 ) ;
#14784 = ORIENTED_EDGE ( 'NONE', *, *, #4423, .F. ) ;
#14785 = SURFACE_STYLE_USAGE ( .BOTH. , #13630 ) ;
#14786 = CARTESIAN_POINT ( 'NONE',  ( -9.456839514482961562, 2.659958822950722723, -58.00000000000012079 ) ) ;
#14787 = CARTESIAN_POINT ( 'NONE',  ( 130.4454129427046496, 23.25070940071369563, 13.14990448602692474 ) ) ;
#14788 = LINE ( 'NONE', #6630, #3253 ) ;
#14789 = VERTEX_POINT ( 'NONE', #12048 ) ;
#14790 = DIRECTION ( 'NONE',  ( 0.000000000000000000, 0.000000000000000000, -1.000000000000000000 ) ) ;
#14791 = CIRCLE ( 'NONE', #3734, 2.499999999999995115 ) ;
#14792 = VECTOR ( 'NONE', #6258, 1000.000000000000000 ) ;
#14793 = CARTESIAN_POINT ( 'NONE',  ( 32.98177247948689939, -56.83166877439235520, 2.758334070755382950 ) ) ;
#14794 = CARTESIAN_POINT ( 'NONE',  ( 56.13062797998802722, -6.952138427283281352, 60.61639468829817190 ) ) ;
#14795 = CARTESIAN_POINT ( 'NONE',  ( -24.99086469133269617, -6.390485686409522081, -48.00342231809331395 ) ) ;
#14796 = VERTEX_POINT ( 'NONE', #1511 ) ;
#14797 = DIRECTION ( 'NONE',  ( -0.000000000000000000, -0.000000000000000000, 1.000000000000000000 ) ) ;
#14798 = AXIS2_PLACEMENT_3D ( 'NONE', #8880, #872, #9119 ) ;
#14799 = VERTEX_POINT ( 'NONE', #1727 ) ;
#14800 = LINE ( 'NONE', #4493, #11332 ) ;
#14801 = PLANE ( 'NONE',  #13815 ) ;
#14802 = VECTOR ( 'NONE', #12097, 1000.000000000000000 ) ;
#14803 = ORIENTED_EDGE ( 'NONE', *, *, #351, .T. ) ;
#14804 = CARTESIAN_POINT ( 'NONE',  ( 65.00000000000001421, -85.24929059928629727, -17.50000000000000000 ) ) ;
#14805 = CARTESIAN_POINT ( 'NONE',  ( 80.00000000000001421, -85.24929059928629727, -32.00000000000000000 ) ) ;
#14806 = EDGE_CURVE ( 'NONE', #14173, #14421, #10044, .T. ) ;
#14807 = EDGE_CURVE ( 'NONE', #15152, #12155, #9457, .T. ) ;
#14808 = AXIS2_PLACEMENT_3D ( 'NONE', #9734, #1564, #1630 ) ;
#14809 = CARTESIAN_POINT ( 'NONE',  ( 12.96675353036119738, -65.20845675887582615, 3.989712384462641204 ) ) ;
#14810 = B_SPLINE_CURVE_WITH_KNOTS ( 'NONE', 3,
 ( #9350, #10806, #10581, #1412, #2644, #1102, #13043, #7263, #7186, #9665 ),
 .UNSPECIFIED., .F., .F.,
 ( 4, 2, 2, 2, 4 ),
 ( 4.399029233930689259E-17, 0.0004995983118108281032, 0.0009991966236216121879, 0.001498794935432396164, 0.001998393247243180140 ),
 .UNSPECIFIED. ) ;
#14811 = CARTESIAN_POINT ( 'NONE',  ( 9.624670876293347277, -53.24145049768178950, 2.425475548247288948 ) ) ;
#14812 = DIRECTION ( 'NONE',  ( 0.000000000000000000, 1.000000000000000000, -0.000000000000000000 ) ) ;
#14813 = PRODUCT_DEFINITION_SHAPE ( 'NONE', 'NONE',  #905 ) ;
#14814 = CIRCLE ( 'NONE', #2539, 9.000000000000001776 ) ;
#14815 = DIRECTION ( 'NONE',  ( 0.000000000000000000, -1.000000000000000000, 0.000000000000000000 ) ) ;
#14816 = CARTESIAN_POINT ( 'NONE',  ( -23.85820543185402798, 3.853856159079054322, -48.12676452506695313 ) ) ;
#14817 = AXIS2_PLACEMENT_3D ( 'NONE', #11776, #3839, #3918 ) ;
#14818 = ORIENTED_EDGE ( 'NONE', *, *, #5591, .T. ) ;
#14819 = CARTESIAN_POINT ( 'NONE',  ( 114.0000000000000284, 19.25070940071369563, -33.00000000000014211 ) ) ;
#14820 = ORIENTED_EDGE ( 'NONE', *, *, #9001, .F. ) ;
#14821 = CARTESIAN_POINT ( 'NONE',  ( 109.8334623555409735, 21.75070940071366365, 139.1143251403882459 ) ) ;
#14822 = VERTEX_POINT ( 'NONE', #13286 ) ;
#14823 = DIRECTION ( 'NONE',  ( 0.8420378618367675427, 0.5394184268574490071, -0.000000000000000000 ) ) ;
#14824 = EDGE_CURVE ( 'NONE', #3324, #6435, #11608, .T. ) ;
#14825 = EDGE_CURVE ( 'NONE', #12456, #10618, #7438, .T. ) ;
#14826 = PLANE ( 'NONE',  #630 ) ;
#14827 = CIRCLE ( 'NONE', #12371, 7.000000000000000000 ) ;
#14828 = DIRECTION ( 'NONE',  ( 1.000000000000000000, 0.000000000000000000, 0.000000000000000000 ) ) ;
#14829 = DIRECTION ( 'NONE',  ( -0.000000000000000000, 1.000000000000000000, -0.000000000000000000 ) ) ;
#14830 = VERTEX_POINT ( 'NONE', #5127 ) ;
#14831 = VECTOR ( 'NONE', #1825, 1000.000000000000000 ) ;
#14832 = FACE_OUTER_BOUND ( 'NONE', #14843, .T. ) ;
#14833 = ORIENTED_EDGE ( 'NONE', *, *, #5655, .F. ) ;
#14834 = CARTESIAN_POINT ( 'NONE',  ( 66.24913411760721260, -11.54048735118959002, 76.19766410831375936 ) ) ;
#14835 = CARTESIAN_POINT ( 'NONE',  ( 8.788876864333699857, -56.07566194134416548, -2.832314198476005629 ) ) ;
#14836 = CARTESIAN_POINT ( 'NONE',  ( -65.00000000000001421, -85.24929059928631148, 19.99999999999999645 ) ) ;
#14837 = CARTESIAN_POINT ( 'NONE',  ( 54.85055839958032209, 21.75070940071329417, 139.1143251403882459 ) ) ;
#14838 = ORIENTED_EDGE ( 'NONE', *, *, #3630, .F. ) ;
#14839 = CARTESIAN_POINT ( 'NONE',  ( 47.27423575335444639, 25.52935533987996664, -33.00000000000012790 ) ) ;
#14840 = VERTEX_POINT ( 'NONE', #9828 ) ;
#14841 = DIRECTION ( 'NONE',  ( -0.8208219420614786266, 0.4549890321264269399, 0.3453061251629920281 ) ) ;
#14842 = ORIENTED_EDGE ( 'NONE', *, *, #1843, .T. ) ;
#14843 = EDGE_LOOP ( 'NONE', ( #1930, #7471, #4771, #13285 ) ) ;
#14844 = CONTEXT_DEPENDENT_SHAPE_REPRESENTATION ( #12237, #9020 ) ;
#14845 = DIRECTION ( 'NONE',  ( 0.000000000000000000, -1.734723475976817547E-15, 1.000000000000000000 ) ) ;
#14846 = CARTESIAN_POINT ( 'NONE',  ( -23.95855436784179560, 3.468451880982295954, -47.93156476714377590 ) ) ;
#14847 = CARTESIAN_POINT ( 'NONE',  ( 11.54983932419131243, -53.31455134687481490, -3.969134470563519645 ) ) ;
#14848 = ORIENTED_EDGE ( 'NONE', *, *, #14629, .F. ) ;
#14849 = FACE_OUTER_BOUND ( 'NONE', #518, .T. ) ;
#14850 = CARTESIAN_POINT ( 'NONE',  ( 33.59732214446785292, -57.16036077483331468, -1.814506011343099523 ) ) ;
#14851 = CARTESIAN_POINT ( 'NONE',  ( 13.39143123690972281, -66.31583591551519419, -4.137138225905224509 ) ) ;
#14852 = EDGE_CURVE ( 'NONE', #788, #4378, #8657, .T. ) ;
#14853 = ORIENTED_EDGE ( 'NONE', *, *, #3435, .F. ) ;
#14854 = CARTESIAN_POINT ( 'NONE',  ( 69.99597282625204286, -3.221539741904409837, 72.92829229118105161 ) ) ;
#14855 = EDGE_CURVE ( 'NONE', #8583, #14121, #1659, .T. ) ;
#14856 = ADVANCED_FACE ( 'NONE', ( #497 ), #5747, .F. ) ;
#14857 = DIRECTION ( 'NONE',  ( 1.000000000000000000, 1.156482317317871725E-16, -0.000000000000000000 ) ) ;
#14858 = ORIENTED_EDGE ( 'NONE', *, *, #2750, .F. ) ;
#14859 = CARTESIAN_POINT ( 'NONE',  ( 28.61048634131497792, -64.14571591460358491, -4.111538053172250073 ) ) ;
#14860 = FACE_OUTER_BOUND ( 'NONE', #13239, .T. ) ;
#14861 =( LENGTH_UNIT ( ) NAMED_UNIT ( * ) SI_UNIT ( .MILLI., .METRE. ) );
#14862 = LINE ( 'NONE', #12485, #9551 ) ;
#14863 = CARTESIAN_POINT ( 'NONE',  ( 27.55953187330915810, 21.75070940071309167, 33.00000000000012790 ) ) ;
#14864 = VERTEX_POINT ( 'NONE', #11409 ) ;
#14865 = CARTESIAN_POINT ( 'NONE',  ( -8.842479278987921631, -7.118053859731281463, 47.50000000000012079 ) ) ;
#14866 = EDGE_CURVE ( 'NONE', #12474, #4665, #11490, .T. ) ;
#14867 = EDGE_CURVE ( 'NONE', #9708, #13714, #8903, .T. ) ;
#14868 = CARTESIAN_POINT ( 'NONE',  ( 47.27423575335444639, 23.25070940071368852, -33.00000000000012790 ) ) ;
#14869 = CARTESIAN_POINT ( 'NONE',  ( 32.82077387253592349, -55.58469383501343941, 2.908670588548392999 ) ) ;
#14870 = CARTESIAN_POINT ( 'NONE',  ( -16.99999999999998579, -12.24929059928630437, 33.00000000000012790 ) ) ;
#14871 = LINE ( 'NONE', #9027, #9634 ) ;
#14872 = ORIENTED_EDGE ( 'NONE', *, *, #1694, .F. ) ;
#14873 = ORIENTED_EDGE ( 'NONE', *, *, #8949, .T. ) ;
#14874 = CARTESIAN_POINT ( 'NONE',  ( 73.69809405469877106, 29.52935533987996664, -21.00807340887166674 ) ) ;
#14875 = EDGE_LOOP ( 'NONE', ( #11418, #3606, #8734, #7617 ) ) ;
#14876 = FACE_BOUND ( 'NONE', #11489, .T. ) ;
#14877 = DIRECTION ( 'NONE',  ( 1.000000000000000000, 0.000000000000000000, 0.000000000000000000 ) ) ;
#14878 = VERTEX_POINT ( 'NONE', #947 ) ;
#14879 = DIRECTION ( 'NONE',  ( 0.8746197071345569451, -0.4848096202550666312, 0.000000000000000000 ) ) ;
#14880 = FACE_OUTER_BOUND ( 'NONE', #14913, .T. ) ;
#14881 = APPLICATION_CONTEXT ( 'automotive_design' ) ;
#14882 = CARTESIAN_POINT ( 'NONE',  ( -32.80254285330622110, -2.278009980413881141, 58.00000000000012079 ) ) ;
#14883 = B_SPLINE_CURVE_WITH_KNOTS ( 'NONE', 3,
 ( #10856, #3695, #91, #316 ),
 .UNSPECIFIED., .F., .F.,
 ( 4, 4 ),
 ( 0.000000000000000000, 0.001771361151111836311 ),
 .UNSPECIFIED. ) ;
#14884 = AXIS2_PLACEMENT_3D ( 'NONE', #7248, #5884, #8265 ) ;
#14885 = LINE ( 'NONE', #6730, #12974 ) ;
#14886 = DIRECTION ( 'NONE',  ( 0.000000000000000000, 1.000000000000000000, -0.000000000000000000 ) ) ;
#14887 = DIRECTION ( 'NONE',  ( -1.000000000000000000, -8.673617379884035472E-17, 0.000000000000000000 ) ) ;
#14888 = EDGE_CURVE ( 'NONE', #2618, #5069, #11333, .T. ) ;
#14889 = DIRECTION ( 'NONE',  ( -0.000000000000000000, -1.000000000000000000, -0.000000000000000000 ) ) ;
#14890 = ORIENTED_EDGE ( 'NONE', *, *, #6126, .F. ) ;
#14891 = CARTESIAN_POINT ( 'NONE',  ( 18.61871093201827421, -52.24929059928630437, -5.564967562786278243 ) ) ;
#14892 = ORIENTED_EDGE ( 'NONE', *, *, #1361, .F. ) ;
#14893 = CARTESIAN_POINT ( 'NONE',  ( 58.00000000000000711, -12.24929059928630970, 38.00000000000012079 ) ) ;
#14894 = AXIS2_PLACEMENT_3D ( 'NONE', #11298, #6530, #9075 ) ;
#14895 = ORIENTED_EDGE ( 'NONE', *, *, #6244, .T. ) ;
#14896 = CARTESIAN_POINT ( 'NONE',  ( 14.38963276113425138, -69.39711819508849544, -4.502057496415714510 ) ) ;
#14897 = AXIS2_PLACEMENT_3D ( 'NONE', #12437, #1890, #6590 ) ;
#14898 = DIRECTION ( 'NONE',  ( 0.000000000000000000, 1.000000000000000000, -0.000000000000000000 ) ) ;
#14899 = DIRECTION ( 'NONE',  ( 0.000000000000000000, 0.000000000000000000, 1.000000000000000000 ) ) ;
#14900 = CARTESIAN_POINT ( 'NONE',  ( 80.00000000000001421, -85.24929059928629727, 8.000000000000001776 ) ) ;
#14901 = DIRECTION ( 'NONE',  ( 0.5006040828730246028, -0.8656763553493059815, 0.000000000000000000 ) ) ;
#14902 = EDGE_LOOP ( 'NONE', ( #7529, #13480, #7133, #7145 ) ) ;
#14903 = VECTOR ( 'NONE', #2815, 1000.000000000000000 ) ;
#14904 = CARTESIAN_POINT ( 'NONE',  ( 65.13162939602318602, -11.91918766459985157, 75.27488260206156667 ) ) ;
#14905 = CARTESIAN_POINT ( 'NONE',  ( 8.756240387056642760, -56.32851134755706113, -2.801743212233170688 ) ) ;
#14906 = DIRECTION ( 'NONE',  ( 0.000000000000000000, 0.000000000000000000, -1.000000000000000000 ) ) ;
#14907 = EDGE_CURVE ( 'NONE', #13146, #5437, #11259, .T. ) ;
#14908 = CARTESIAN_POINT ( 'NONE',  ( -11.57001547143821085, -9.459140135624386048, 48.26605223432068925 ) ) ;
#14909 = ORIENTED_EDGE ( 'NONE', *, *, #5178, .F. ) ;
#14910 = ORIENTED_EDGE ( 'NONE', *, *, #8013, .T. ) ;
#14911 = CARTESIAN_POINT ( 'NONE',  ( -24.54316048551696028, -7.158540021523408292, -58.00000000000012079 ) ) ;
#14912 = AXIS2_PLACEMENT_3D ( 'NONE', #4039, #9913, #7745 ) ;
#14913 = EDGE_LOOP ( 'NONE', ( #14433, #3956, #1274, #2158 ) ) ;
#14914 = DIRECTION ( 'NONE',  ( -1.000000000000000000, -1.156482317317870492E-16, 0.000000000000000000 ) ) ;
#14915 = AXIS2_PLACEMENT_3D ( 'NONE', #9667, #5174, #12027 ) ;
#14916 = ORIENTED_EDGE ( 'NONE', *, *, #55, .F. ) ;
#14917 = PRODUCT_DEFINITION_SHAPE ( 'NONE', 'NONE',  #15237 ) ;
#14918 = AXIS2_PLACEMENT_3D ( 'NONE', #11452, #10087, #5627 ) ;
#14919 = ORIENTED_EDGE ( 'NONE', *, *, #1119, .T. ) ;
#14920 = CIRCLE ( 'NONE', #5333, 0.4999999999999999445 ) ;
#14921 = DIRECTION ( 'NONE',  ( -0.4848096202550659650, -0.8746197071345572782, 0.000000000000000000 ) ) ;
#14922 = CARTESIAN_POINT ( 'NONE',  ( -22.44582411025819368, 4.950411932228481859, -48.32458034485718912 ) ) ;
#14923 = VERTEX_POINT ( 'NONE', #12500 ) ;
#14924 = DIRECTION ( 'NONE',  ( -0.000000000000000000, -0.000000000000000000, -1.000000000000000000 ) ) ;
#14925 = DIRECTION ( 'NONE',  ( -0.8420378618367728718, -0.5394184268574404584, -0.000000000000000000 ) ) ;
#14926 = ORIENTED_EDGE ( 'NONE', *, *, #4967, .F. ) ;
#14927 = VECTOR ( 'NONE', #7449, 1000.000000000000000 ) ;
#14928 = PRODUCT_DEFINITION_FORMATION_WITH_SPECIFIED_SOURCE ( 'ANY', '', #14949, .NOT_KNOWN. ) ;
#14929 = EDGE_CURVE ( 'NONE', #5523, #1026, #2190, .T. ) ;
#14930 = CARTESIAN_POINT ( 'NONE',  ( 76.00751999314820750, -6.514251586541772276, 73.19766410831374515 ) ) ;
#14931 = CARTESIAN_POINT ( 'NONE',  ( 69.37814714961265850, -3.660029812082665313, 77.09164763542320031 ) ) ;
#14932 = CIRCLE ( 'NONE', #1666, 31.00000000000000000 ) ;
#14933 = DIRECTION ( 'NONE',  ( -0.000000000000000000, 0.000000000000000000, -1.000000000000000000 ) ) ;
#14934 = CARTESIAN_POINT ( 'NONE',  ( 35.08843044364380859, -47.02811197266221654, 2.732446379177822848 ) ) ;
#14935 = AXIS2_PLACEMENT_3D ( 'NONE', #15031, #9189, #13720 ) ;
#14936 = VERTEX_POINT ( 'NONE', #3108 ) ;
#14937 = VECTOR ( 'NONE', #6840, 1000.000000000000000 ) ;
#14938 = CARTESIAN_POINT ( 'NONE',  ( 33.59375882623609044, -57.17378631614185736, 2.501045389179021861 ) ) ;
#14939 = CARTESIAN_POINT ( 'NONE',  ( -8.779641963837230279, 13.70511383897430058, -48.50000000000012079 ) ) ;
#14940 = ORIENTED_EDGE ( 'NONE', *, *, #10960, .T. ) ;
#14941 = CARTESIAN_POINT ( 'NONE',  ( 19.97461805067967333, -82.24929059928629727, 4.000000000000001776 ) ) ;
#14942 = DIRECTION ( 'NONE',  ( 0.000000000000000000, 0.000000000000000000, -1.000000000000000000 ) ) ;
#14943 = VECTOR ( 'NONE', #9305, 1000.000000000000000 ) ;
#14944 = ORIENTED_EDGE ( 'NONE', *, *, #10463, .F. ) ;
#14945 = CARTESIAN_POINT ( 'NONE',  ( -6.999999999999985789, -2.249290599286299930, -32.99999999999994316 ) ) ;
#14946 = EDGE_CURVE ( 'NONE', #307, #4665, #10887, .T. ) ;
#14947 = DIRECTION ( 'NONE',  ( -0.000000000000000000, -0.000000000000000000, -1.000000000000000000 ) ) ;
#14948 = ORIENTED_EDGE ( 'NONE', *, *, #13357, .T. ) ;
#14949 = PRODUCT ( 'L-Shaped Aluminum Bracket', 'L-Shaped Aluminum Bracket', '', ( #13171 ) ) ;
#14950 = CONICAL_SURFACE ( 'NONE', #7338, 2.524999999999999467, 0.7853981633973787790 ) ;
#14951 = CARTESIAN_POINT ( 'NONE',  ( -9.198099351547387670, 2.262399358110477543, -48.50000000000012079 ) ) ;
#14952 = CYLINDRICAL_SURFACE ( 'NONE', #4626, 0.7892041907098262810 ) ;
#14953 = LINE ( 'NONE', #4402, #1706 ) ;
#14954 = CARTESIAN_POINT ( 'NONE',  ( 19.97461805067967688, -85.24929059928631148, -4.000000000000000888 ) ) ;
#14955 = FACE_OUTER_BOUND ( 'NONE', #6009, .T. ) ;
#14956 = EDGE_CURVE ( 'NONE', #10712, #6376, #12859, .T. ) ;
#14957 = ORIENTED_EDGE ( 'NONE', *, *, #13545, .T. ) ;
#14958 = ORIENTED_EDGE ( 'NONE', *, *, #15115, .T. ) ;
#14959 = ORIENTED_EDGE ( 'NONE', *, *, #6175, .T. ) ;
#14960 = EDGE_CURVE ( 'NONE', #10116, #12681, #6568, .T. ) ;
#14961 = CARTESIAN_POINT ( 'NONE',  ( -8.982583014919022446, 1.839844381040865118, -47.50000000000012079 ) ) ;
#14962 = CARTESIAN_POINT ( 'NONE',  ( 8.091875466796901506, -56.24057709915800274, 1.858739038532483123 ) ) ;
#14963 = EDGE_CURVE ( 'NONE', #4994, #3246, #13576, .T. ) ;
#14964 = EDGE_CURVE ( 'NONE', #3249, #1474, #10196, .T. ) ;
#14965 = VERTEX_POINT ( 'NONE', #5422 ) ;
#14966 = DIRECTION ( 'NONE',  ( -0.000000000000000000, 0.000000000000000000, 1.000000000000000000 ) ) ;
#14967 = DIRECTION ( 'NONE',  ( -0.000000000000000000, 1.000000000000000000, -0.000000000000000000 ) ) ;
#14968 = CARTESIAN_POINT ( 'NONE',  ( 10.00023835250150661, -61.42570632716525836, 2.132522520905367980 ) ) ;
#14969 = EDGE_CURVE ( 'NONE', #9315, #5234, #5983, .T. ) ;
#14970 = DIRECTION ( 'NONE',  ( 0.000000000000000000, 0.000000000000000000, 1.000000000000000000 ) ) ;
#14971 = CARTESIAN_POINT ( 'NONE',  ( 32.52281604437752804, -59.06479067038043240, 2.757123406423070744 ) ) ;
#14972 = DIRECTION ( 'NONE',  ( 0.9744556954135545901, 0.2245798247307308204, 0.000000000000000000 ) ) ;
#14973 = CARTESIAN_POINT ( 'NONE',  ( 9.488545476451129446, -59.84602720838573475, 2.809343037843349045 ) ) ;
#14974 = CARTESIAN_POINT ( 'NONE',  ( 58.00000000000000711, -2.249290599286309256, 39.50000000000012790 ) ) ;
#14975 = ORIENTED_EDGE ( 'NONE', *, *, #12415, .T. ) ;
#14976 = CARTESIAN_POINT ( 'NONE',  ( 93.56770215592470663, 23.25070940071369208, 139.1143251403882459 ) ) ;
#14977 = ORIENTED_EDGE ( 'NONE', *, *, #9628, .T. ) ;
#14978 = VECTOR ( 'NONE', #7406, 1000.000000000000000 ) ;
#14979 = DIRECTION ( 'NONE',  ( 0.000000000000000000, 0.000000000000000000, -1.000000000000000000 ) ) ;
#14980 = PRESENTATION_LAYER_ASSIGNMENT (  '', '', ( #6378 ) ) ;
#14981 = EDGE_LOOP ( 'NONE', ( #871, #12218, #10641, #14106 ) ) ;
#14982 = CARTESIAN_POINT ( 'NONE',  ( 12.22773363228717614, -62.74876579108499897, -3.782929430830273443 ) ) ;
#14983 = EDGE_CURVE ( 'NONE', #1809, #1117, #4331, .T. ) ;
#14984 = CARTESIAN_POINT ( 'NONE',  ( -2.016677571526633510E-15, 23.25070940071368497, 139.1143251403882459 ) ) ;
#14985 = DIRECTION ( 'NONE',  ( 0.000000000000000000, -0.000000000000000000, -1.000000000000000000 ) ) ;
#14986 = CARTESIAN_POINT ( 'NONE',  ( 21.74884261173415467, -96.56299909827106376, 4.000000000000001776 ) ) ;
#14987 = ADVANCED_FACE ( 'NONE', ( #11569 ), #3185, .T. ) ;
#14988 = DIRECTION ( 'NONE',  ( -0.000000000000000000, -0.000000000000000000, -1.000000000000000000 ) ) ;
#14989 = ORIENTED_EDGE ( 'NONE', *, *, #2924, .T. ) ;
#14990 = CIRCLE ( 'NONE', #8369, 7.000000000000000000 ) ;
#14991 = LINE ( 'NONE', #2134, #5400 ) ;
#14992 = CARTESIAN_POINT ( 'NONE',  ( 8.199792978590132009, -57.47994873761392398, -2.501453769636599045 ) ) ;
#14993 = CARTESIAN_POINT ( 'NONE',  ( 56.59738969056744651, 23.25070940071368852, 33.00000000000012790 ) ) ;
#14994 = LINE ( 'NONE', #13912, #14357 ) ;
#14995 = VERTEX_POINT ( 'NONE', #4497 ) ;
#14996 = VERTEX_POINT ( 'NONE', #9202 ) ;
#14997 = DIRECTION ( 'NONE',  ( 1.000000000000000000, 0.000000000000000000, 0.000000000000000000 ) ) ;
#14998 = ORIENTED_EDGE ( 'NONE', *, *, #13486, .T. ) ;
#14999 = DIRECTION ( 'NONE',  ( 0.000000000000000000, 1.000000000000000000, -0.000000000000000000 ) ) ;
#15000 = VERTEX_POINT ( 'NONE', #12581 ) ;
#15001 = AXIS2_PLACEMENT_3D ( 'NONE', #12369, #1821, #14744 ) ;
#15002 = LINE ( 'NONE', #8923, #1668 ) ;
#15003 = DIRECTION ( 'NONE',  ( 0.000000000000000000, 1.000000000000000000, 0.000000000000000000 ) ) ;
#15005 = ADVANCED_FACE ( 'NONE', ( #5579 ), #1028, .F. ) ;
#15004 = ORIENTED_EDGE ( 'NONE', *, *, #7032, .F. ) ;
#15006 = ADVANCED_FACE ( 'NONE', ( #7735 ), #2104, .F. ) ;
#15007 = DIRECTION ( 'NONE',  ( 0.8908241094534407045, 0.4543483311474627029, 0.000000000000000000 ) ) ;
#15008 = DIRECTION ( 'NONE',  ( 0.000000000000000000, 0.000000000000000000, 1.000000000000000000 ) ) ;
#15009 = ORIENTED_EDGE ( 'NONE', *, *, #5025, .T. ) ;
#15010 = AXIS2_PLACEMENT_3D ( 'NONE', #9744, #2722, #12118 ) ;
#15011 = CARTESIAN_POINT ( 'NONE',  ( 80.00000000000001421, -87.24929059928631148, -35.00000000000000000 ) ) ;
#15012 = FACE_OUTER_BOUND ( 'NONE', #2433, .T. ) ;
#15013 = FACE_BOUND ( 'NONE', #10559, .T. ) ;
#15014 = CARTESIAN_POINT ( 'NONE',  ( 52.72873328492558187, -0.5014548242779810483, 60.61639468829817190 ) ) ;
#15015 = CARTESIAN_POINT ( 'NONE',  ( -65.00000000000001421, -87.24929059928631148, 17.50000000000000000 ) ) ;
#15016 = ORIENTED_EDGE ( 'NONE', *, *, #11389, .F. ) ;
#15017 = CARTESIAN_POINT ( 'NONE',  ( 70.22813770118101218, -4.160309161658024557, 72.22283181065139956 ) ) ;
#15018 = LINE ( 'NONE', #3087, #5671 ) ;
#15019 = VECTOR ( 'NONE', #7829, 1000.000000000000000 ) ;
#15020 = VERTEX_POINT ( 'NONE', #8039 ) ;
#15021 = DIRECTION ( 'NONE',  ( 1.000000000000000000, 0.000000000000000000, 0.000000000000000000 ) ) ;
#15022 = DIRECTION ( 'NONE',  ( -0.000000000000000000, 1.000000000000000000, -0.000000000000000000 ) ) ;
#15023 = ADVANCED_FACE ( 'NONE', ( #14273 ), #15122, .T. ) ;
#15024 = AXIS2_PLACEMENT_3D ( 'NONE', #6845, #14013, #9244 ) ;
#15025 = ADVANCED_FACE ( 'NONE', ( #11651 ), #7189, .T. ) ;
#15026 = LINE ( 'NONE', #11546, #11488 ) ;
#15027 = CARTESIAN_POINT ( 'NONE',  ( -9.875903985900572835, 2.387222743937554181, -57.50000000000012079 ) ) ;
#15028 = VERTEX_POINT ( 'NONE', #5816 ) ;
#15029 = DIRECTION ( 'NONE',  ( 0.000000000000000000, 0.000000000000000000, 1.000000000000000000 ) ) ;
#15030 = AXIS2_PLACEMENT_3D ( 'NONE', #711, #7806, #5505 ) ;
#15031 = CARTESIAN_POINT ( 'NONE',  ( 58.00000000000000711, -2.249290599286309256, 39.50000000000012790 ) ) ;
#15032 = CARTESIAN_POINT ( 'NONE',  ( 31.30110669430510129, -53.71233130651034315, 3.555899869131480706 ) ) ;
#15033 = CIRCLE ( 'NONE', #8883, 2.499999999999995115 ) ;
#15034 = PLANE ( 'NONE',  #12770 ) ;
#15035 = CARTESIAN_POINT ( 'NONE',  ( 80.00000000000001421, -72.24929059928631148, -32.99999999999999289 ) ) ;
#15036 = AXIS2_PLACEMENT_3D ( 'NONE', #12977, #11732, #4654 ) ;
#15037 = ORIENTED_EDGE ( 'NONE', *, *, #13357, .F. ) ;
#15038 = CARTESIAN_POINT ( 'NONE',  ( 31.96811279043434340, -60.26979819505955760, 2.885043711492953467 ) ) ;
#15039 = ORIENTED_EDGE ( 'NONE', *, *, #7164, .F. ) ;
#15040 = FACE_BOUND ( 'NONE', #2547, .T. ) ;
#15041 = CARTESIAN_POINT ( 'NONE',  ( -3.190546569013415379, 0.8906624217387615339, -48.00000000000012079 ) ) ;
#15042 = EDGE_LOOP ( 'NONE', ( #9527, #10687 ) ) ;
#15043 = TOROIDAL_SURFACE ( 'NONE', #1534, 7.924024642120688355, 1.000000000000000000 ) ;
#15044 = DIRECTION ( 'NONE',  ( 0.000000000000000000, 0.000000000000000000, 1.000000000000000000 ) ) ;
#15045 = CARTESIAN_POINT ( 'NONE',  ( 24.62796245282055452, -82.24929059928629727, -1.347403282660978752 ) ) ;
#15046 = VECTOR ( 'NONE', #712, 1000.000000000000114 ) ;
#15047 = VECTOR ( 'NONE', #4619, 1000.000000000000000 ) ;
#15048 = CARTESIAN_POINT ( 'NONE',  ( 84.72310019870096198, 29.52935533987996664, -33.00000000000013500 ) ) ;
#15049 = ADVANCED_FACE ( 'NONE', ( #1259 ), #10729, .T. ) ;
#15050 = DIRECTION ( 'NONE',  ( -0.8746197071345570562, 0.4848096202550665756, 0.000000000000000000 ) ) ;
#15051 = CARTESIAN_POINT ( 'NONE',  ( 31.62073844763337149, -60.61171897230391892, 3.004288329735560925 ) ) ;
#15052 = LINE ( 'NONE', #10435, #9372 ) ;
#15053 = CARTESIAN_POINT ( 'NONE',  ( 62.35557539207178479, -5.694598376804811402, 60.61639468829817190 ) ) ;
#15054 = CIRCLE ( 'NONE', #1546, 10.46463184759104692 ) ;
#15055 = CIRCLE ( 'NONE', #508, 1.000000000000000000 ) ;
#15056 = PLANE ( 'NONE',  #11480 ) ;
#15057 = VECTOR ( 'NONE', #1244, 1000.000000000000000 ) ;
#15058 = ORIENTED_EDGE ( 'NONE', *, *, #10927, .F. ) ;
#15059 = CARTESIAN_POINT ( 'NONE',  ( 8.859806296821686189, -57.78392871910184425, -2.727962224264455227 ) ) ;
#15060 = CIRCLE ( 'NONE', #4016, 4.999999999999997335 ) ;
#15061 = EDGE_LOOP ( 'NONE', ( #8092, #11831, #5268, #8259 ) ) ;
#15062 = EDGE_CURVE ( 'NONE', #12456, #5927, #5973, .T. ) ;
#15063 = LINE ( 'NONE', #5597, #4441 ) ;
#15064 = EDGE_LOOP ( 'NONE', ( #8195, #4024, #9160, #13293 ) ) ;
#15065 = CARTESIAN_POINT ( 'NONE',  ( 13.47628073630851731, -64.89641169172402613, -4.245552436241592176 ) ) ;
#15066 = CARTESIAN_POINT ( 'NONE',  ( 17.87818865416384995, -64.01730164816855506, -6.333338579777395339 ) ) ;
#15067 = VECTOR ( 'NONE', #7886, 1000.000000000000000 ) ;
#15068 = DIRECTION ( 'NONE',  ( -0.000000000000000000, 1.000000000000000000, 0.000000000000000000 ) ) ;
#15069 = CARTESIAN_POINT ( 'NONE',  ( 18.61871093201827065, -52.24929059928630437, -5.564967562786285349 ) ) ;
#15070 = VECTOR ( 'NONE', #13364, 1000.000000000000000 ) ;
#15071 = VERTEX_POINT ( 'NONE', #3572 ) ;
#15072 = CIRCLE ( 'NONE', #11872, 3.999999999999999112 ) ;
#15073 = EDGE_CURVE ( 'NONE', #1083, #11420, #8118, .T. ) ;
#15074 = EDGE_CURVE ( 'NONE', #1691, #65, #120, .T. ) ;
#15075 = CARTESIAN_POINT ( 'NONE',  ( 65.83900612928935914, -11.71016173102437818, 76.08636588808168710 ) ) ;
#15076 = CARTESIAN_POINT ( 'NONE',  ( 8.142427707716008101, -55.84923954203681973, -1.895000442031717913 ) ) ;
#15077 = CARTESIAN_POINT ( 'NONE',  ( 54.00000000000000711, -2.249290599286311032, 38.00000000000012079 ) ) ;
#15078 = CARTESIAN_POINT ( 'NONE',  ( -11.04362772831848716, -9.031687326780717839, 48.03392779025379156 ) ) ;
#15079 = ORIENTED_EDGE ( 'NONE', *, *, #901, .T. ) ;
#15080 = DIRECTION ( 'NONE',  ( 0.000000000000000000, 0.000000000000000000, -1.000000000000000000 ) ) ;
#15081 = ORIENTED_EDGE ( 'NONE', *, *, #7776, .F. ) ;
#15082 = DIRECTION ( 'NONE',  ( -0.3020115420618249003, 0.1674077314120184790, -0.9384901064608620613 ) ) ;
#15083 = ORIENTED_EDGE ( 'NONE', *, *, #431, .T. ) ;
#15084 = CIRCLE ( 'NONE', #3037, 2.500000000000002220 ) ;
#15085 = AXIS2_PLACEMENT_3D ( 'NONE', #10474, #5550, #4545 ) ;
#15086 = ORIENTED_EDGE ( 'NONE', *, *, #3917, .T. ) ;
#15087 = CARTESIAN_POINT ( 'NONE',  ( -9.271822474830662131, -6.861803161813125662, 47.50000000000012079 ) ) ;
#15088 = CARTESIAN_POINT ( 'NONE',  ( 73.69809405469877106, 25.52935533987996664, -21.00807340887166674 ) ) ;
#15089 = DIRECTION ( 'NONE',  ( -0.000000000000000000, -0.000000000000000000, 1.000000000000000000 ) ) ;
#15090 = DIRECTION ( 'NONE',  ( 0.000000000000000000, 1.000000000000000000, -0.000000000000000000 ) ) ;
#15091 = VERTEX_POINT ( 'NONE', #9505 ) ;
#15092 = CARTESIAN_POINT ( 'NONE',  ( 20.86173033120691045, -53.24929059928630437, 0.000000000000000000 ) ) ;
#15093 = CARTESIAN_POINT ( 'NONE',  ( 50.01091543003727224, 23.25070940071368852, -33.00000000000012790 ) ) ;
#15094 = CARTESIAN_POINT ( 'NONE',  ( 33.60245346892040885, -55.93345933723782792, -2.599599694949141337 ) ) ;
#15095 = CARTESIAN_POINT ( 'NONE',  ( 23.47858629692699495, -52.24929059928630437, 6.492462156583981958 ) ) ;
#15096 = CARTESIAN_POINT ( 'NONE',  ( 31.77253520366416950, -63.13950256936100658, 2.713503986087918651 ) ) ;
#15097 = ORIENTED_EDGE ( 'NONE', *, *, #1365, .F. ) ;
#15098 = CARTESIAN_POINT ( 'NONE',  ( 69.39833270110392505, -3.557321787083441489, 72.23228168306333430 ) ) ;
#15099 = EDGE_CURVE ( 'NONE', #14405, #6921, #14123, .T. ) ;
#15100 = DIRECTION ( 'NONE',  ( -0.000000000000000000, 1.000000000000000000, -0.000000000000000000 ) ) ;
#15101 = ADVANCED_FACE ( 'NONE', ( #7036 ), #6043, .F. ) ;
#15102 = ORIENTED_EDGE ( 'NONE', *, *, #11525, .T. ) ;
#15103 = LINE ( 'NONE', #13943, #11344 ) ;
#15104 = CARTESIAN_POINT ( 'NONE',  ( 58.00000000000000711, -2.249290599286309256, 72.19766410831374515 ) ) ;
#15105 = LINE ( 'NONE', #3323, #8655 ) ;
#15106 = ORIENTED_EDGE ( 'NONE', *, *, #12758, .F. ) ;
#15107 = ORIENTED_EDGE ( 'NONE', *, *, #14122, .F. ) ;
#15108 = DIRECTION ( 'NONE',  ( 1.000000000000000000, 0.000000000000000000, 0.000000000000000000 ) ) ;
#15109 = PLANE ( 'NONE',  #9878 ) ;
#15110 = FACE_OUTER_BOUND ( 'NONE', #12714, .T. ) ;
#15111 = PLANE ( 'NONE',  #2193 ) ;
#15112 = CARTESIAN_POINT ( 'NONE',  ( 18.61871093201827421, -52.24929059928630437, -5.564967562786278243 ) ) ;
#15113 = CARTESIAN_POINT ( 'NONE',  ( 121.5907739023289622, -31.78146182366518957, 56.28371344025897827 ) ) ;
#15114 = EDGE_CURVE ( 'NONE', #5252, #1527, #13121, .T. ) ;
#15115 = EDGE_CURVE ( 'NONE', #12295, #12778, #3758, .T. ) ;
#15116 = VERTEX_POINT ( 'NONE', #12901 ) ;
#15117 = CARTESIAN_POINT ( 'NONE',  ( 24.36188411769309781, -73.69234276600508338, -6.062089035220971311 ) ) ;
#15118 = ORIENTED_EDGE ( 'NONE', *, *, #3409, .F. ) ;
#15119 = DIRECTION ( 'NONE',  ( -0.000000000000000000, -0.000000000000000000, -1.000000000000000000 ) ) ;
#15120 = DIRECTION ( 'NONE',  ( 0.000000000000000000, 0.000000000000000000, 1.000000000000000000 ) ) ;
#15121 = ORIENTED_EDGE ( 'NONE', *, *, #7083, .F. ) ;
#15122 = CYLINDRICAL_SURFACE ( 'NONE', #553, 0.7892041907098262810 ) ;
#15123 = DIRECTION ( 'NONE',  ( 0.8656763553492640151, 0.5006040828730974335, 0.000000000000000000 ) ) ;
#15124 = DIRECTION ( 'NONE',  ( 1.000000000000000000, 0.000000000000000000, 0.000000000000000000 ) ) ;
#15125 = SHAPE_REPRESENTATION ( 'MAS-317', ( #9785, #7795, #1156, #9775, #6080, #10994, #11726, #6800, #13689, #4342, #14657 ), #4095 ) ;
#15126 = CARTESIAN_POINT ( 'NONE',  ( 52.50499674461036648, -3.053107681157296582, 54.56811043785582882 ) ) ;
#15127 = LINE ( 'NONE', #3661, #12751 ) ;
#15128 = CYLINDRICAL_SURFACE ( 'NONE', #13299, 1.000000000000000888 ) ;
#15129 = EDGE_CURVE ( 'NONE', #12366, #12204, #2344, .T. ) ;
#15130 = DIRECTION ( 'NONE',  ( 1.000000000000000000, 0.000000000000000000, 0.000000000000000000 ) ) ;
#15131 = LINE ( 'NONE', #7823, #916 ) ;
#15132 = ORIENTED_EDGE ( 'NONE', *, *, #11952, .F. ) ;
#15133 = CARTESIAN_POINT ( 'NONE',  ( 12.93509704890846557, -54.57042255619801097, -4.214900875586402584 ) ) ;
#15134 = ORIENTED_EDGE ( 'NONE', *, *, #13548, .F. ) ;
#15135 = CARTESIAN_POINT ( 'NONE',  ( 8.201103799357262858, -57.48563641131178770, 1.816685854991387794 ) ) ;
#15136 = ORIENTED_EDGE ( 'NONE', *, *, #12236, .F. ) ;
#15137 = CARTESIAN_POINT ( 'NONE',  ( 27.80179776399110736, -69.39711819508849544, 3.972674503026243809 ) ) ;
#15138 = LINE ( 'NONE', #5767, #171 ) ;
#15139 = AXIS2_PLACEMENT_3D ( 'NONE', #12643, #4316, #11397 ) ;
#15140 = CARTESIAN_POINT ( 'NONE',  ( 13.15381962123460191, -65.59433601606468756, -3.409308316089461055 ) ) ;
#15141 = ORIENTED_EDGE ( 'NONE', *, *, #10897, .F. ) ;
#15142 = EDGE_CURVE ( 'NONE', #3601, #9272, #8205, .T. ) ;
#15143 = DIRECTION ( 'NONE',  ( 0.000000000000000000, 0.000000000000000000, 1.000000000000000000 ) ) ;
#15144 = CARTESIAN_POINT ( 'NONE',  ( 8.128335720592605895, -55.93948076112146595, -2.601440957440732227 ) ) ;
#15145 = DIRECTION ( 'NONE',  ( 0.8746197071345569451, -0.4848096202550666312, 0.000000000000000000 ) ) ;
#15146 = CARTESIAN_POINT ( 'NONE',  ( -10.12835026901530178, -8.341055813471566438, 48.12459668492476084 ) ) ;
#15147 = EDGE_LOOP ( 'NONE', ( #13137, #6862, #11087, #6619 ) ) ;
#15148 = AXIS2_PLACEMENT_3D ( 'NONE', #3702, #2400, #11861 ) ;
#15149 = CARTESIAN_POINT ( 'NONE',  ( -25.21252699837112132, -6.998437922861946880, 48.50000000000012079 ) ) ;
#15150 = ORIENTED_EDGE ( 'NONE', *, *, #10509, .F. ) ;
#15151 = CARTESIAN_POINT ( 'NONE',  ( -8.787473001628837821, 2.499856724289235554, 57.50000000000012079 ) ) ;
#15152 = VERTEX_POINT ( 'NONE', #11728 ) ;
#15153 = ORIENTED_EDGE ( 'NONE', *, *, #12379, .F. ) ;
#15154 = EDGE_CURVE ( 'NONE', #5063, #13149, #6553, .T. ) ;
#15155 = EDGE_CURVE ( 'NONE', #11686, #14069, #5896, .T. ) ;
#15156 = LINE ( 'NONE', #10771, #4113 ) ;
#15157 = LINE ( 'NONE', #10772, #5508 ) ;
#15158 = AXIS2_PLACEMENT_3D ( 'NONE', #8743, #5070, #9776 ) ;
#15159 = DIRECTION ( 'NONE',  ( 1.000000000000000000, 0.000000000000000000, 0.000000000000000000 ) ) ;
#15160 = VECTOR ( 'NONE', #11491, 1000.000000000000000 ) ;
#15161 = CARTESIAN_POINT ( 'NONE',  ( -80.00000000000001421, -76.24929059928631148, 6.000000000000000000 ) ) ;
#15162 = ORIENTED_EDGE ( 'NONE', *, *, #1810, .T. ) ;
#15163 = ADVANCED_FACE ( 'NONE', ( #2425 ), #7264, .T. ) ;
#15164 = DIRECTION ( 'NONE',  ( 0.000000000000000000, 1.000000000000000000, 0.000000000000000000 ) ) ;
#15165 = CARTESIAN_POINT ( 'NONE',  ( 62.70356846721307420, -0.3817325368051065482, 48.51982618741349285 ) ) ;
#15166 = VECTOR ( 'NONE', #4372, 1000.000000000000000 ) ;
#15167 = DIRECTION ( 'NONE',  ( 0.8208219420614786266, -0.4549890321264268289, -0.3453061251629919726 ) ) ;
#15168 = CARTESIAN_POINT ( 'NONE',  ( 58.00000000000000711, -2.249290599286311032, 38.00000000000012079 ) ) ;
#15169 = ORIENTED_EDGE ( 'NONE', *, *, #12225, .T. ) ;
#15170 = CARTESIAN_POINT ( 'NONE',  ( 108.0866310645538562, 23.25070940071369563, 13.14990448602692474 ) ) ;
#15171 = EDGE_CURVE ( 'NONE', #3763, #2576, #11801, .T. ) ;
#15172 = CIRCLE ( 'NONE', #1884, 8.924024642120691908 ) ;
#15173 = ORIENTED_EDGE ( 'NONE', *, *, #6572, .T. ) ;
#15174 = DIRECTION ( 'NONE',  ( 0.3020115420618249003, -0.1674077314120184790, 0.9384901064608621724 ) ) ;
#15175 = EDGE_LOOP ( 'NONE', ( #15220, #12914, #3822, #6257 ) ) ;
#15176 =( NAMED_UNIT ( * ) SI_UNIT ( $, .STERADIAN. ) SOLID_ANGLE_UNIT ( ) );
#15177 = DIRECTION ( 'NONE',  ( -0.000000000000000000, -0.000000000000000000, 1.000000000000000000 ) ) ;
#15178 = PLANE ( 'NONE',  #4482 ) ;
#15179 = ORIENTED_EDGE ( 'NONE', *, *, #14675, .T. ) ;
#15180 = AXIS2_PLACEMENT_3D ( 'NONE', #9909, #1734, #13509 ) ;
#15181 = PRODUCT_DEFINITION_FORMATION_WITH_SPECIFIED_SOURCE ( 'ANY', '', #675, .NOT_KNOWN. ) ;
#15182 = FACE_OUTER_BOUND ( 'NONE', #13983, .T. ) ;
#15183 = DIRECTION ( 'NONE',  ( -0.000000000000000000, 1.000000000000000000, -0.000000000000000000 ) ) ;
#15184 = TOROIDAL_SURFACE ( 'NONE', #1652, 6.000000000000000000, 1.000000000000000000 ) ;
#15185 = EDGE_CURVE ( 'NONE', #12155, #5046, #9273, .T. ) ;
#15186 = VECTOR ( 'NONE', #1007, 1000.000000000000000 ) ;
#15187 = CARTESIAN_POINT ( 'NONE',  ( 10.00023835250150483, -61.42570632716525125, 2.500000000000000000 ) ) ;
#15188 = CARTESIAN_POINT ( 'NONE',  ( 61.36510378087922390, 1.530577915148011225, 62.84860122826521689 ) ) ;
#15189 = LINE ( 'NONE', #6787, #13995 ) ;
#15190 = DIRECTION ( 'NONE',  ( 1.000000000000000000, 0.000000000000000000, 0.000000000000000000 ) ) ;
#15191 = VERTEX_POINT ( 'NONE', #5259 ) ;
#15192 = DIRECTION ( 'NONE',  ( 0.000000000000000000, 0.000000000000000000, 1.000000000000000000 ) ) ;
#15193 = ORIENTED_EDGE ( 'NONE', *, *, #13924, .T. ) ;
#15194 = CARTESIAN_POINT ( 'NONE',  ( 56.25419740419757630, 3.022649838004307199, 48.51982618741349285 ) ) ;
#15195 = CARTESIAN_POINT ( 'NONE',  ( 13.86173033120691223, -69.39711819508849544, 2.500000000000000000 ) ) ;
#15196 = AXIS2_PLACEMENT_3D ( 'NONE', #1482, #109, #10533 ) ;
#15197 = ORIENTED_EDGE ( 'NONE', *, *, #6685, .F. ) ;
#15198 = DIRECTION ( 'NONE',  ( 0.000000000000000000, -0.000000000000000000, -1.000000000000000000 ) ) ;
#15199 = DIRECTION ( 'NONE',  ( -0.000000000000000000, 1.927470528863120035E-16, 1.000000000000000000 ) ) ;
#15200 = EDGE_CURVE ( 'NONE', #14923, #3720, #10241, .T. ) ;
#15201 = ADVANCED_FACE ( 'NONE', ( #267 ), #14424, .T. ) ;
#15202 = CARTESIAN_POINT ( 'NONE',  ( 53.04398595309534414, -1.224959495890951100, 62.84860122826521689 ) ) ;
#15203 = CARTESIAN_POINT ( 'NONE',  ( 96.29968967959054282, 25.52935533987996664, 84.20452624982236500 ) ) ;
#15204 = DIRECTION ( 'NONE',  ( -0.000000000000000000, -0.000000000000000000, -1.000000000000000000 ) ) ;
#15205 = CARTESIAN_POINT ( 'NONE',  ( -24.96222495693456978, -7.431276100536581275, 58.00000000000012079 ) ) ;
#15206 = CARTESIAN_POINT ( 'NONE',  ( 31.78593137074030395, -54.06014836395551271, 3.368555242453529885 ) ) ;
#15207 = ORIENTED_EDGE ( 'NONE', *, *, #5554, .F. ) ;
#15208 = CARTESIAN_POINT ( 'NONE',  ( 18.00340353970562646, -60.79495753919547241, -6.390225278801568543 ) ) ;
#15209 = UNCERTAINTY_MEASURE_WITH_UNIT (LENGTH_MEASURE( 1.000000000000000082E-05 ), #9484, 'distance_accuracy_value', 'NONE');
#15210 = ORIENTED_EDGE ( 'NONE', *, *, #2323, .F. ) ;
#15211 = DIRECTION ( 'NONE',  ( 1.000000000000000000, 0.000000000000000000, 0.000000000000000000 ) ) ;
#15212 = ORIENTED_EDGE ( 'NONE', *, *, #11377, .T. ) ;
#15213 = LINE ( 'NONE', #7903, #2474 ) ;
#15214 = ORIENTED_EDGE ( 'NONE', *, *, #1475, .F. ) ;
#15215 = CARTESIAN_POINT ( 'NONE',  ( 12.36791015745245836, -56.52532528994181860, 2.500000000000000000 ) ) ;
#15216 =( BOUNDED_SURFACE ( )  B_SPLINE_SURFACE ( 3, 2, ( 
 ( #11808, #8507, #127 ),
 ( #9512, #13051, #9596 ),
 ( #14208, #9358, #14049 ),
 ( #12906, #14131, #6050 ),
 ( #7041, #8284, #3511 ),
 ( #2582, #3662, #14278 ),
 ( #48, #7125, #10587 ),
 ( #1421, #274, #12979 ),
 ( #10737, #8362, #1268 ),
 ( #5981, #198, #1198 ) ),
 .UNSPECIFIED., .F., .F., .F. ) 
 B_SPLINE_SURFACE_WITH_KNOTS ( ( 4, 2, 2, 2, 4 ),
 ( 3, 3 ),
 ( 0.0006711510808134562266, 0.001062132081067026709, 0.001453113081320597409, 0.001844094081574168108, 0.002235075081827738591 ),
 ( 0.000000000000000000, 1.000000000000000000 ),
 .UNSPECIFIED. ) 
 GEOMETRIC_REPRESENTATION_ITEM ( )  RATIONAL_B_SPLINE_SURFACE ( (
 ( 1.000000000000000000, 0.7254762501099963901, 1.000000000000000000),
 ( 1.000000000000000000, 0.7255094664176422459, 1.000000000000000000),
 ( 1.000000000000000000, 0.7239949553644952074, 1.000000000000000000),
 ( 1.000000000000000000, 0.7190573720639429345, 1.000000000000000000),
 ( 1.000000000000000000, 0.7156412189950915881, 1.000000000000000000),
 ( 1.000000000000000000, 0.7094102539594338008, 1.000000000000000000),
 ( 1.000000000000000000, 0.7066203625162998936, 1.000000000000000000),
 ( 1.000000000000000000, 0.7042417591947802702, 1.000000000000000000),
 ( 1.000000000000000000, 0.7046402682201203804, 1.000000000000000000),
 ( 1.000000000000000000, 0.7071067811865500152, 1.000000000000000000) ) ) 
 REPRESENTATION_ITEM ( '' )  SURFACE ( )  );
#15217 = EDGE_CURVE ( 'NONE', #15000, #59, #4086, .T. ) ;
#15218 = EDGE_CURVE ( 'NONE', #14513, #11720, #10503, .T. ) ;
#15219 = DIRECTION ( 'NONE',  ( -0.8656763553493062036, -0.5006040828730242698, -0.000000000000000000 ) ) ;
#15220 = ORIENTED_EDGE ( 'NONE', *, *, #12441, .T. ) ;
#15221 = ORIENTED_EDGE ( 'NONE', *, *, #950, .F. ) ;
#15222 = DIRECTION ( 'NONE',  ( 0.000000000000000000, -0.000000000000000000, -1.000000000000000000 ) ) ;
#15223 = DIRECTION ( 'NONE',  ( 0.000000000000000000, 0.000000000000000000, 1.000000000000000000 ) ) ;
#15224 = CARTESIAN_POINT ( 'NONE',  ( 53.81626139532630049, -82.24929059928629727, -11.78977872328356646 ) ) ;
#15225 = DIRECTION ( 'NONE',  ( -0.000000000000000000, 0.000000000000000000, 1.000000000000000000 ) ) ;
#15226 = CIRCLE ( 'NONE', #3676, 2.524999999999999467 ) ;
#15227 = AXIS2_PLACEMENT_3D ( 'NONE', #12631, #1079, #14015 ) ;
#15228 = NEXT_ASSEMBLY_USAGE_OCCURRENCE ( 'NAUO1', ' ', ' ', #10316, #11824, $ ) ;
#15229 = NEXT_ASSEMBLY_USAGE_OCCURRENCE ( 'NAUO2', ' ', ' ', #10316, #3261, $ ) ;
#15230 = NEXT_ASSEMBLY_USAGE_OCCURRENCE ( 'NAUO3', ' ', ' ', #10316, #6372, $ ) ;
#15231 = NEXT_ASSEMBLY_USAGE_OCCURRENCE ( 'NAUO4', ' ', ' ', #10316, #12292, $ ) ;
#15232 = NEXT_ASSEMBLY_USAGE_OCCURRENCE ( 'NAUO5', ' ', ' ', #10316, #905, $ ) ;
#15233 = NEXT_ASSEMBLY_USAGE_OCCURRENCE ( 'NAUO6', ' ', ' ', #10316, #1199, $ ) ;
#15234 = NEXT_ASSEMBLY_USAGE_OCCURRENCE ( 'NAUO7', ' ', ' ', #10316, #9858, $ ) ;
#15235 = NEXT_ASSEMBLY_USAGE_OCCURRENCE ( 'NAUO8', ' ', ' ', #10316, #905, $ ) ;
#15236 = NEXT_ASSEMBLY_USAGE_OCCURRENCE ( 'NAUO9', ' ', ' ', #10316, #5056, $ ) ;
#15237 = NEXT_ASSEMBLY_USAGE_OCCURRENCE ( 'NAUO10', ' ', ' ', #10316, #7585, $ ) ;
#15238=COLOUR_RGB('Dark Blue',0.08,0.2,0.34);
#15239=FILL_AREA_STYLE_COLOUR('',#15238);
#15240=FILL_AREA_STYLE('',(#15239));
#15241=SURFACE_STYLE_FILL_AREA(#15240);
#15242=SURFACE_SIDE_STYLE('',(#15241));
#15243=SURFACE_STYLE_USAGE(.BOTH.,#15242);
#15244=PRESENTATION_STYLE_ASSIGNMENT((#15243));
#15245=COLOUR_RGB('Light Blue',0.38,0.62,0.78);
#15246=FILL_AREA_STYLE_COLOUR('',#15245);
#15247=FILL_AREA_STYLE('',(#15246));
#15248=SURFACE_STYLE_FILL_AREA(#15247);
#15249=SURFACE_SIDE_STYLE('',(#15248));
#15250=SURFACE_STYLE_USAGE(.BOTH.,#15249);
#15251=PRESENTATION_STYLE_ASSIGNMENT((#15250));
#15252=COLOUR_RGB('Sky Blue',0.24,0.69,0.87);
#15253=FILL_AREA_STYLE_COLOUR('',#15252);
#15254=FILL_AREA_STYLE('',(#15253));
#15255=SURFACE_STYLE_FILL_AREA(#15254);
#15256=SURFACE_SIDE_STYLE('',(#15255));
#15257=SURFACE_STYLE_USAGE(.BOTH.,#15256);
#15258=PRESENTATION_STYLE_ASSIGNMENT((#15257));
#15259=COLOUR_RGB('Grey',0.48,0.52,0.57);
#15260=FILL_AREA_STYLE_COLOUR('',#15259);
#15261=FILL_AREA_STYLE('',(#15260));
#15262=SURFACE_STYLE_FILL_AREA(#15261);
#15263=SURFACE_SIDE_STYLE('',(#15262));
#15264=SURFACE_STYLE_USAGE(.BOTH.,#15263);
#15265=PRESENTATION_STYLE_ASSIGNMENT((#15264));
#15266=COLOUR_RGB('Black',0.12,0.14,0.17);
#15267=FILL_AREA_STYLE_COLOUR('',#15266);
#15268=FILL_AREA_STYLE('',(#15267));
#15269=SURFACE_STYLE_FILL_AREA(#15268);
#15270=SURFACE_SIDE_STYLE('',(#15269));
#15271=SURFACE_STYLE_USAGE(.BOTH.,#15270);
#15272=PRESENTATION_STYLE_ASSIGNMENT((#15271));
#15273=COLOUR_RGB('Off White',0.89,0.88,0.83);
#15274=FILL_AREA_STYLE_COLOUR('',#15273);
#15275=FILL_AREA_STYLE('',(#15274));
#15276=SURFACE_STYLE_FILL_AREA(#15275);
#15277=SURFACE_SIDE_STYLE('',(#15276));
#15278=SURFACE_STYLE_USAGE(.BOTH.,#15277);
#15279=PRESENTATION_STYLE_ASSIGNMENT((#15278));
ENDSEC;
END-ISO-10303-21;
